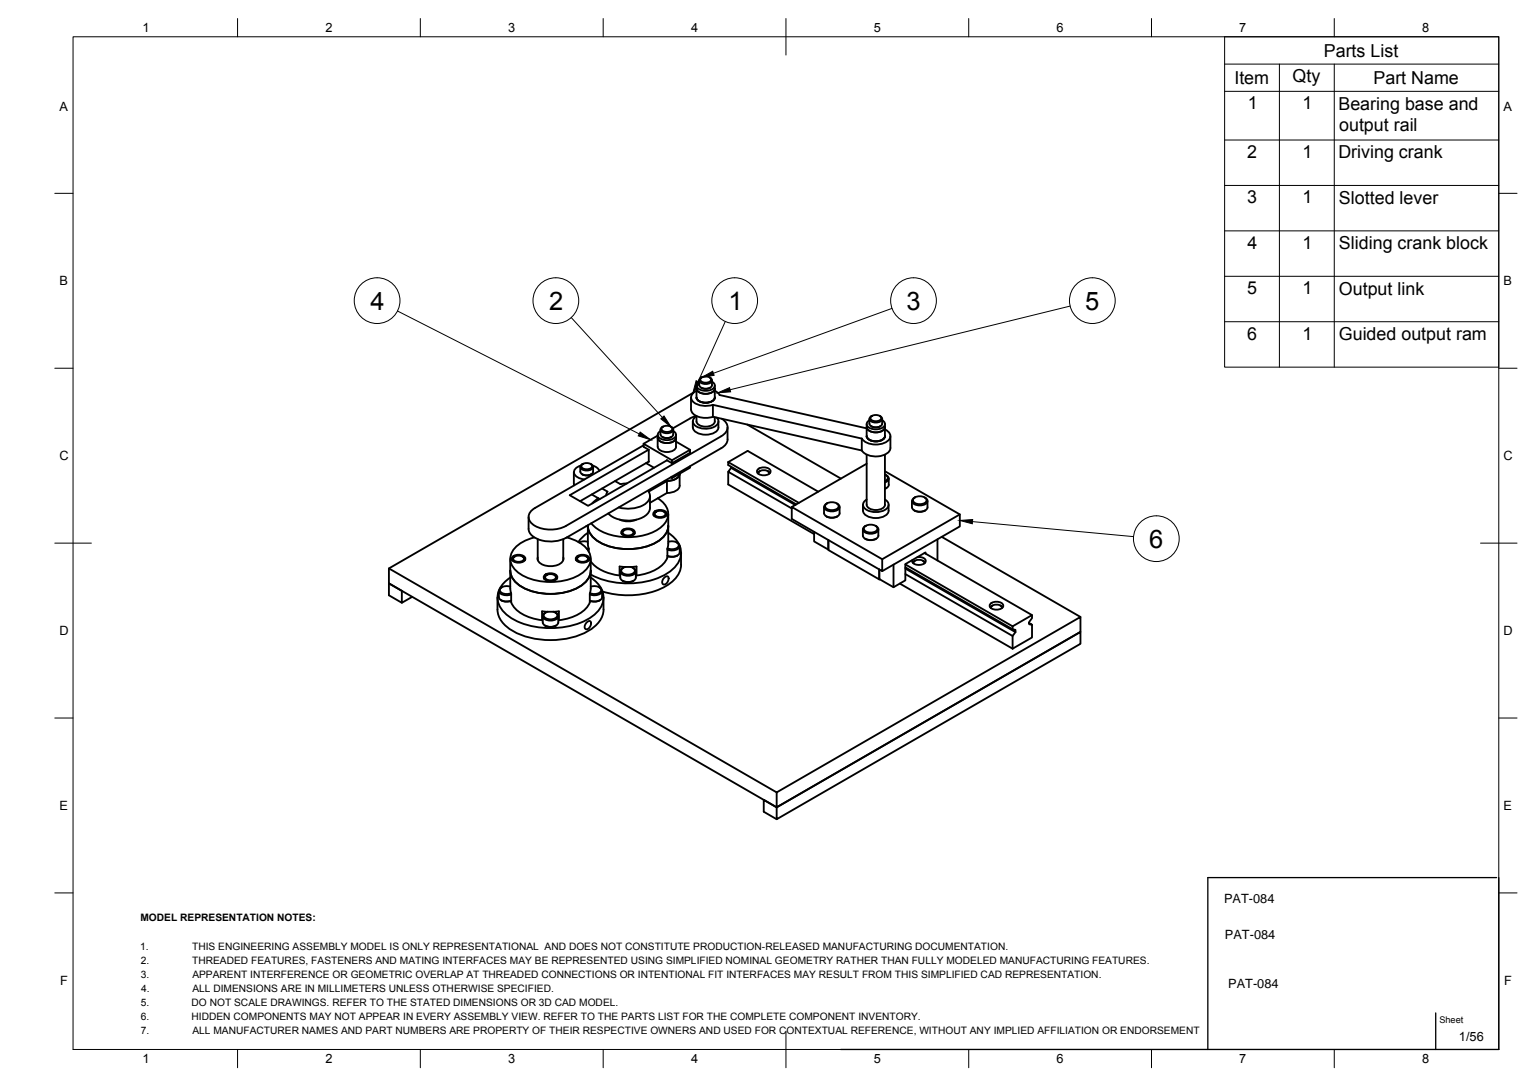
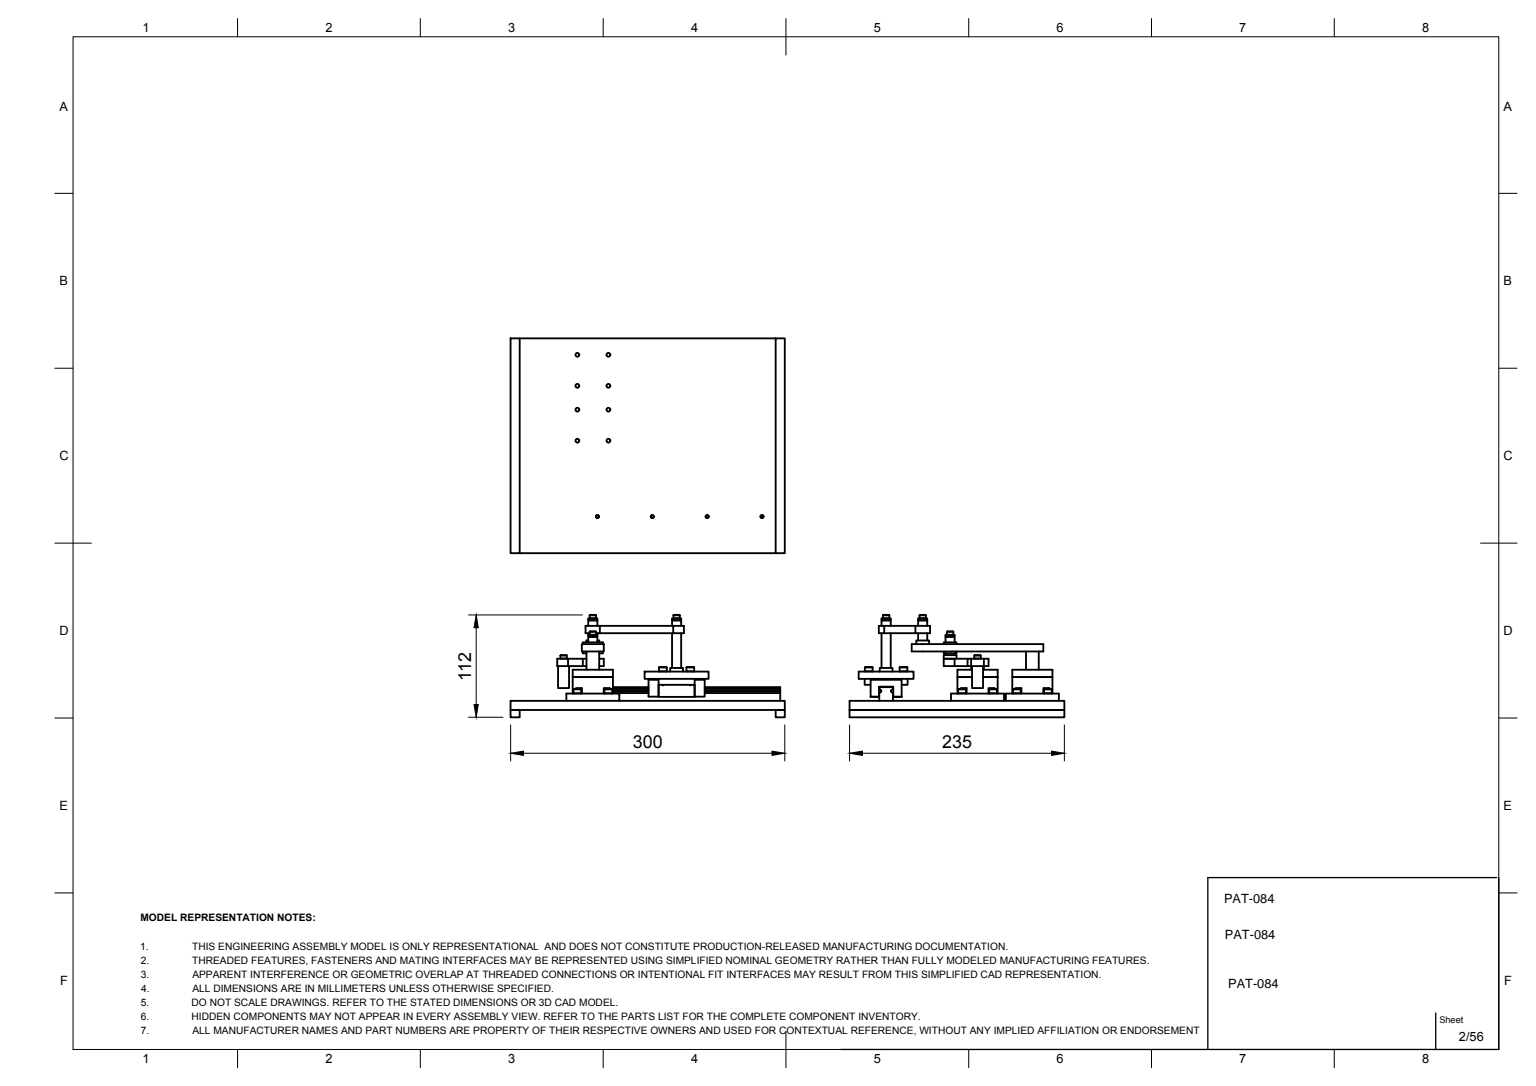
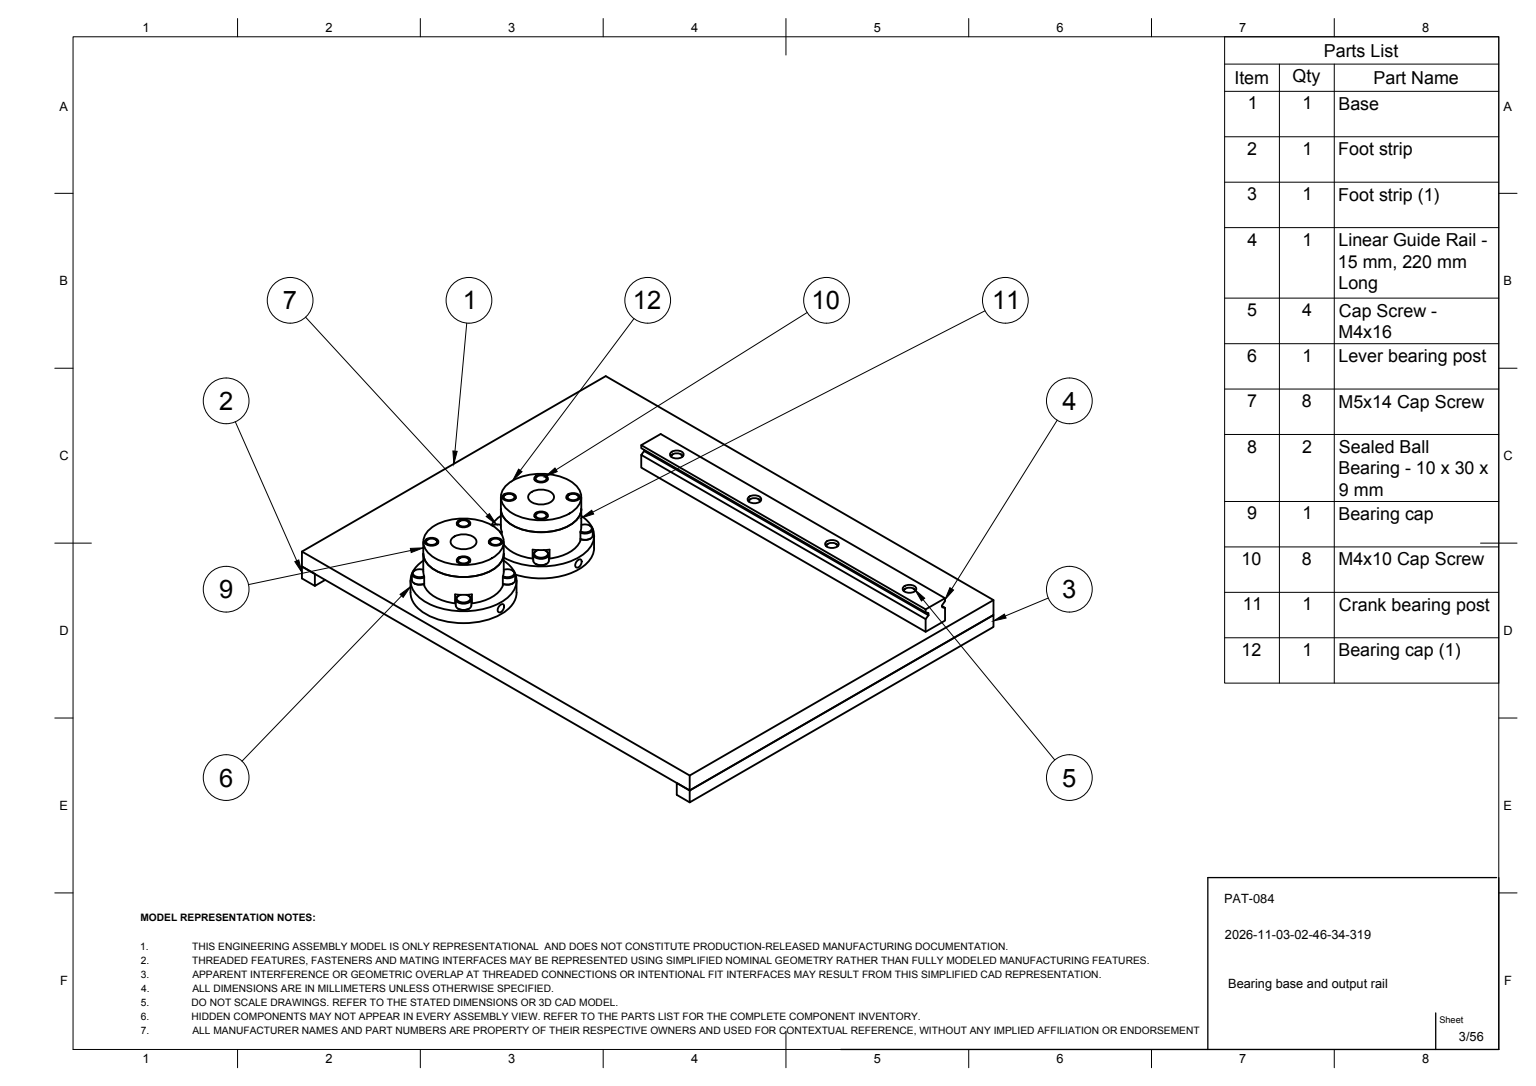
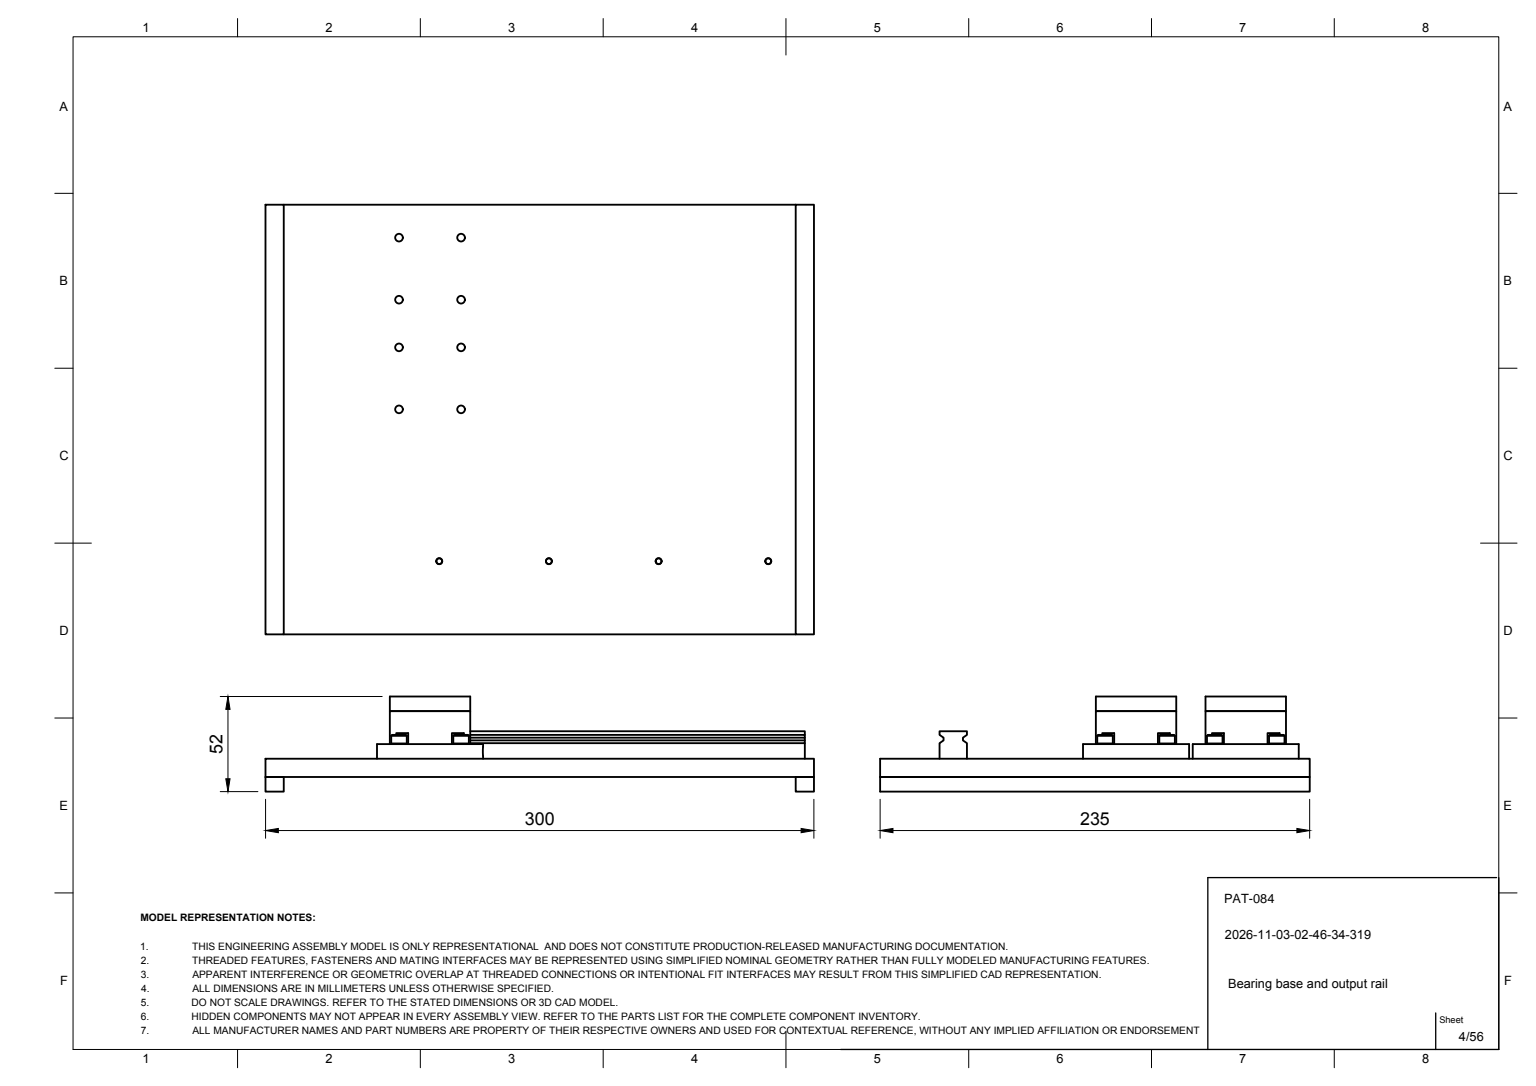
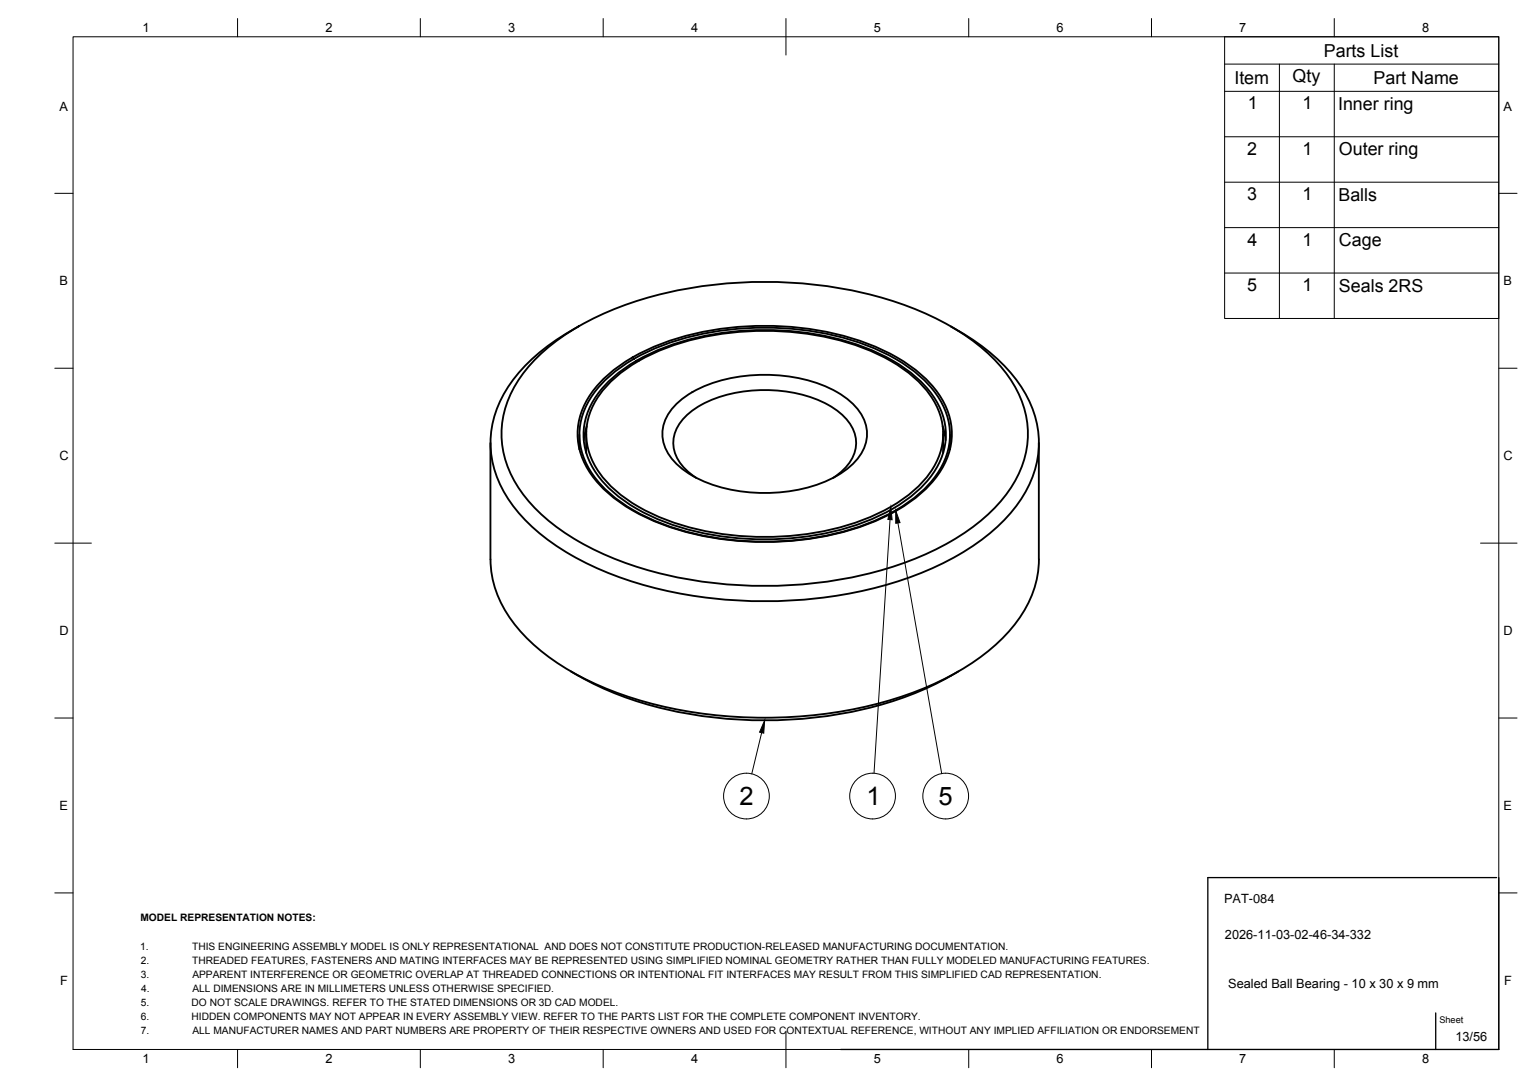
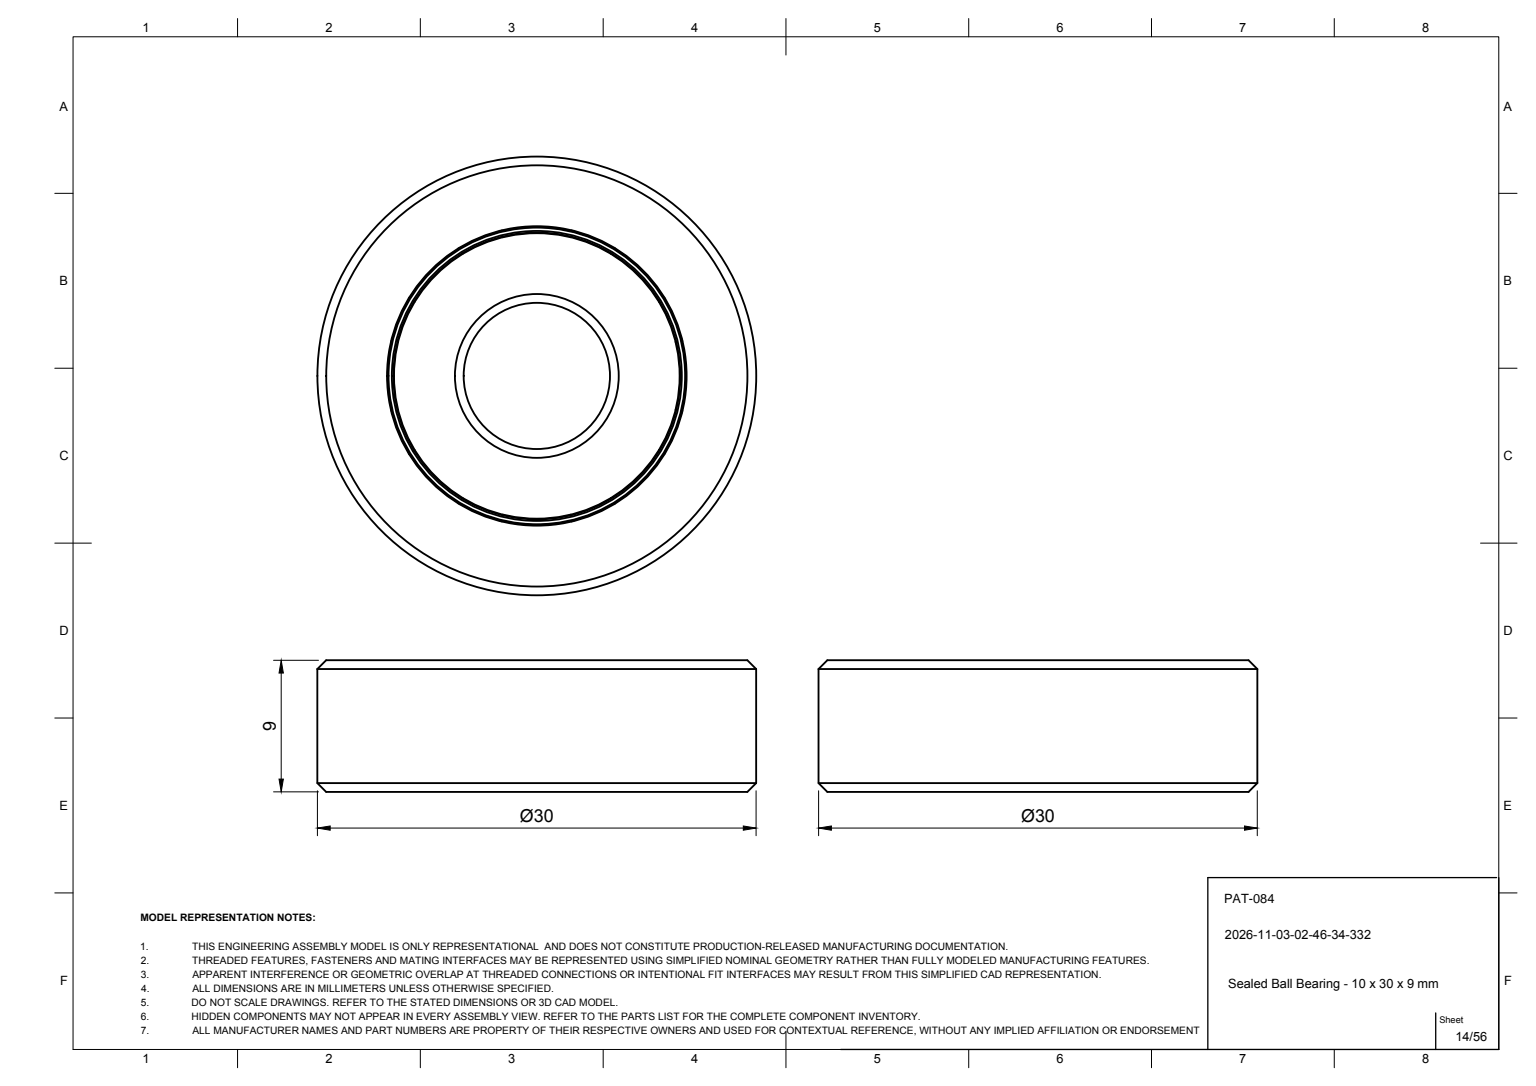
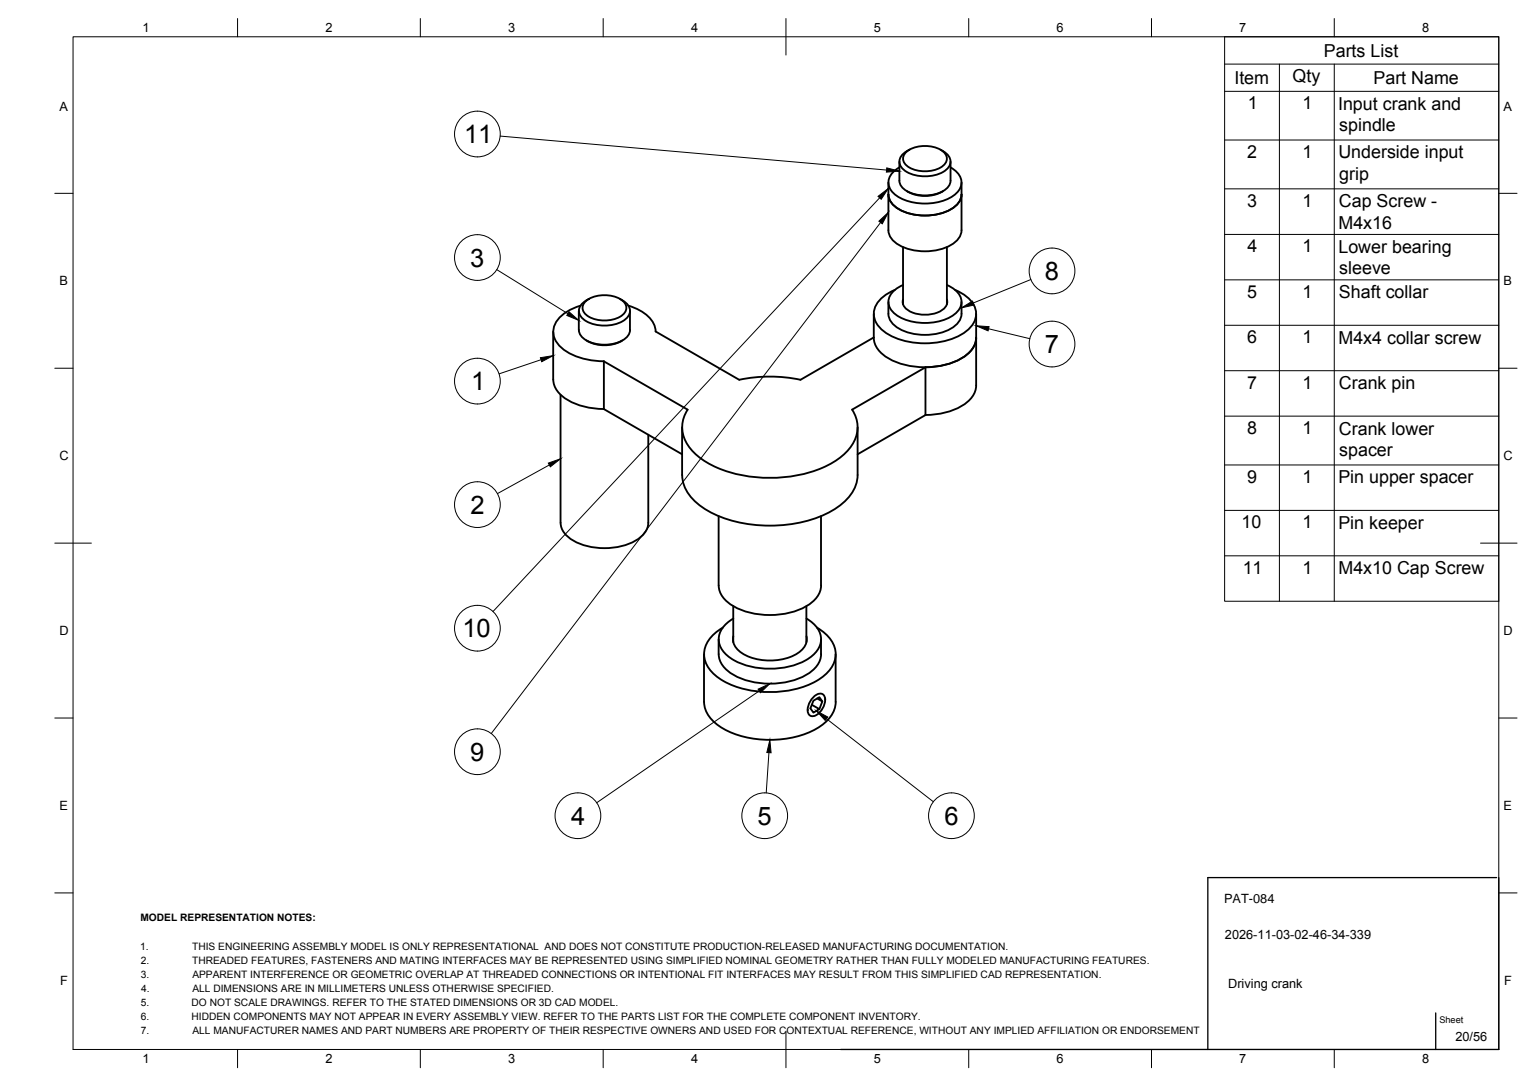
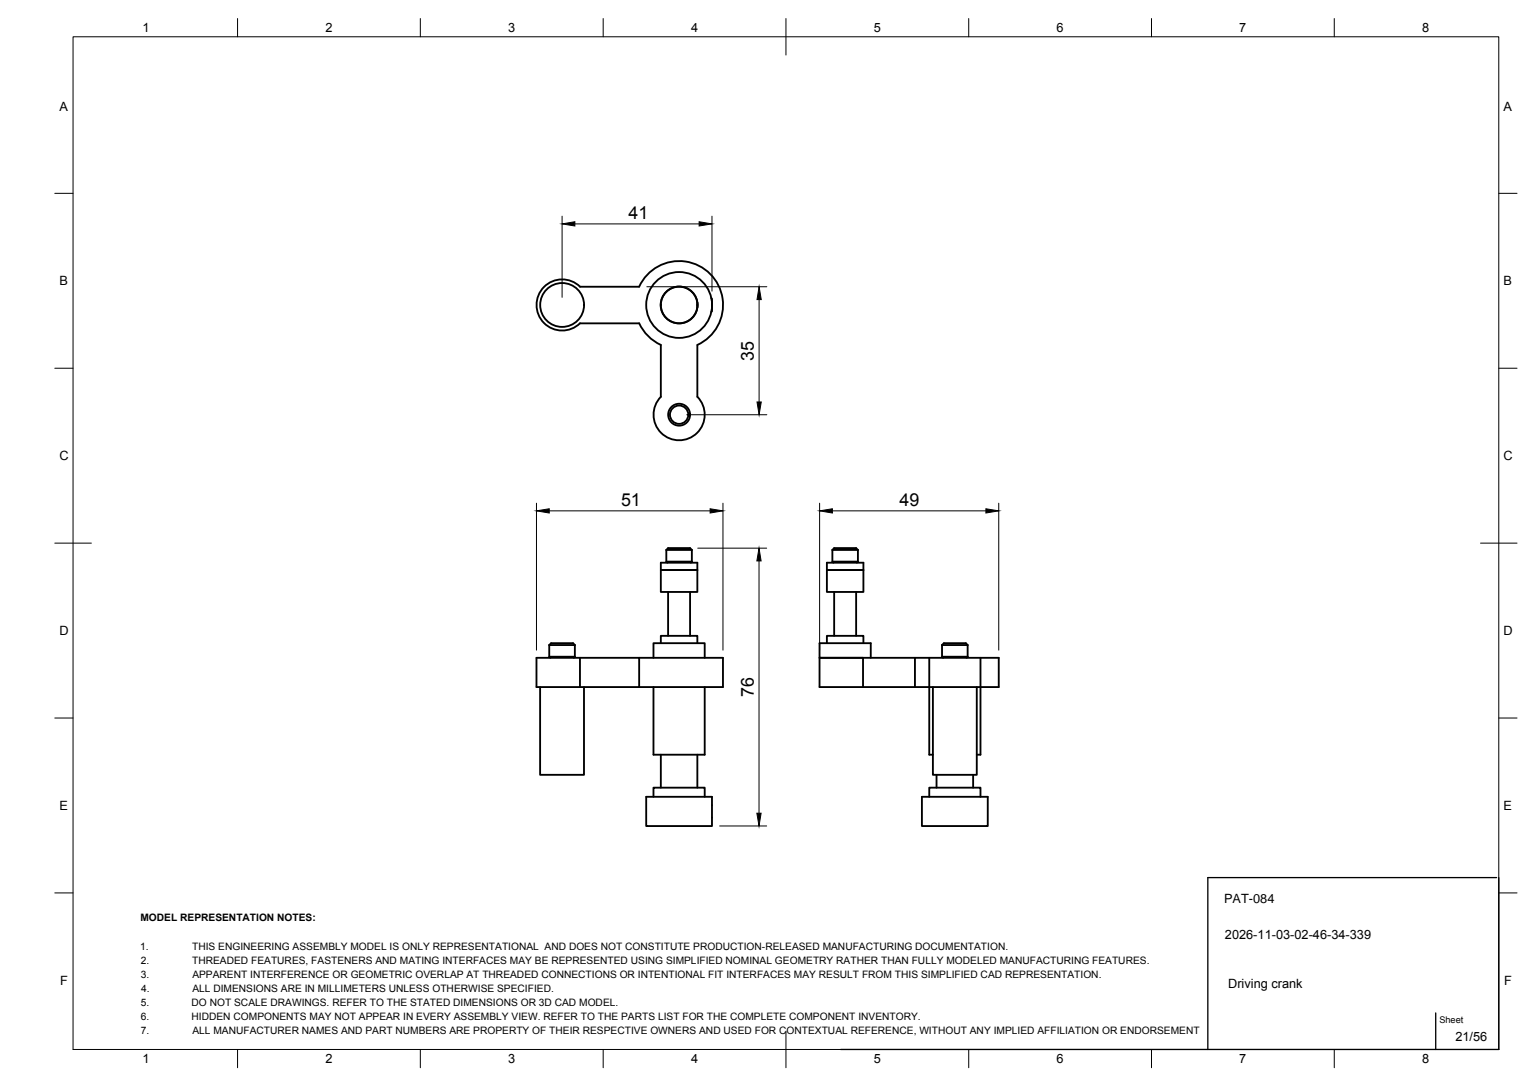
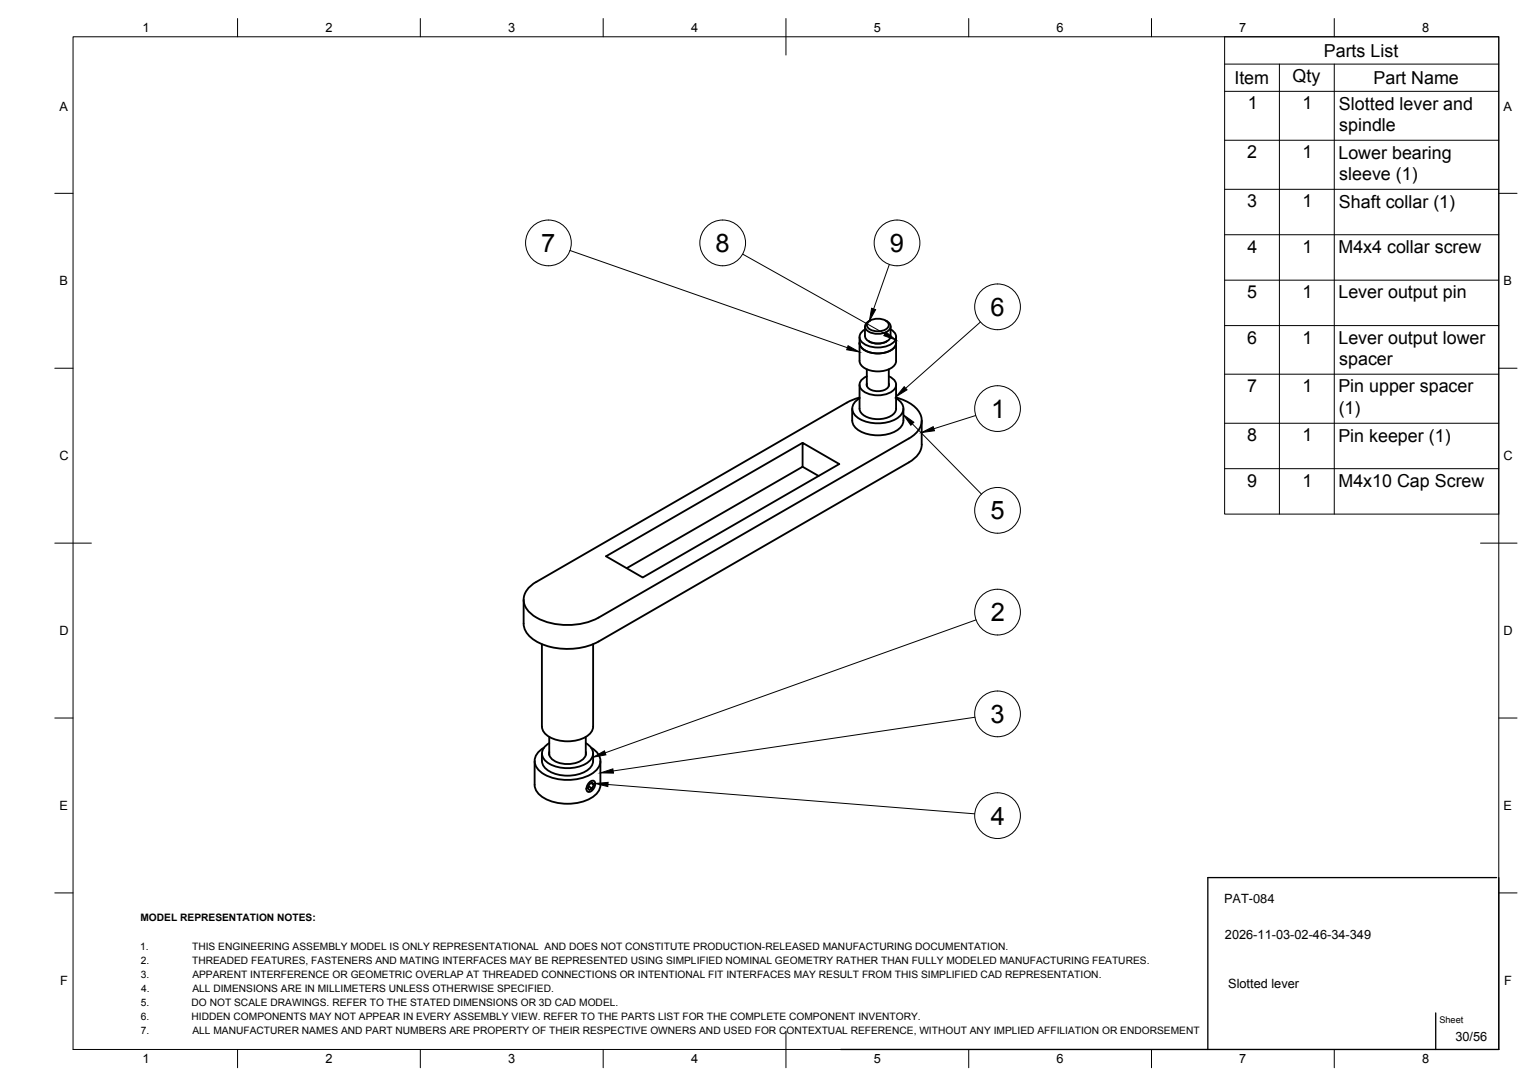
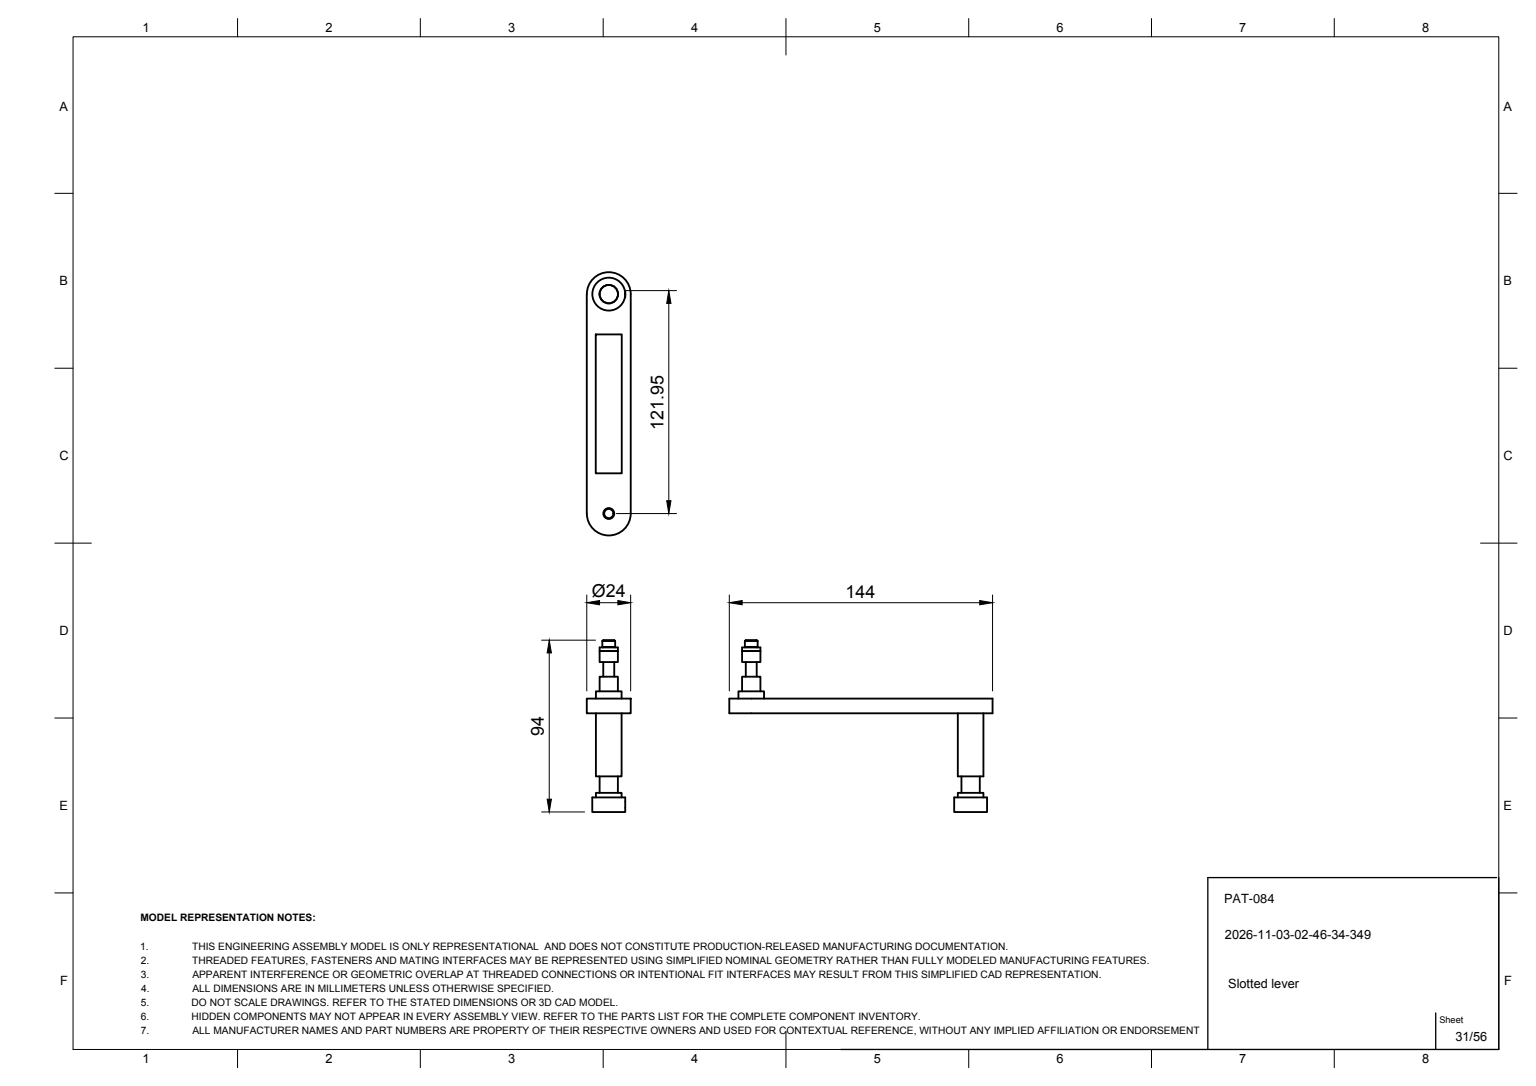
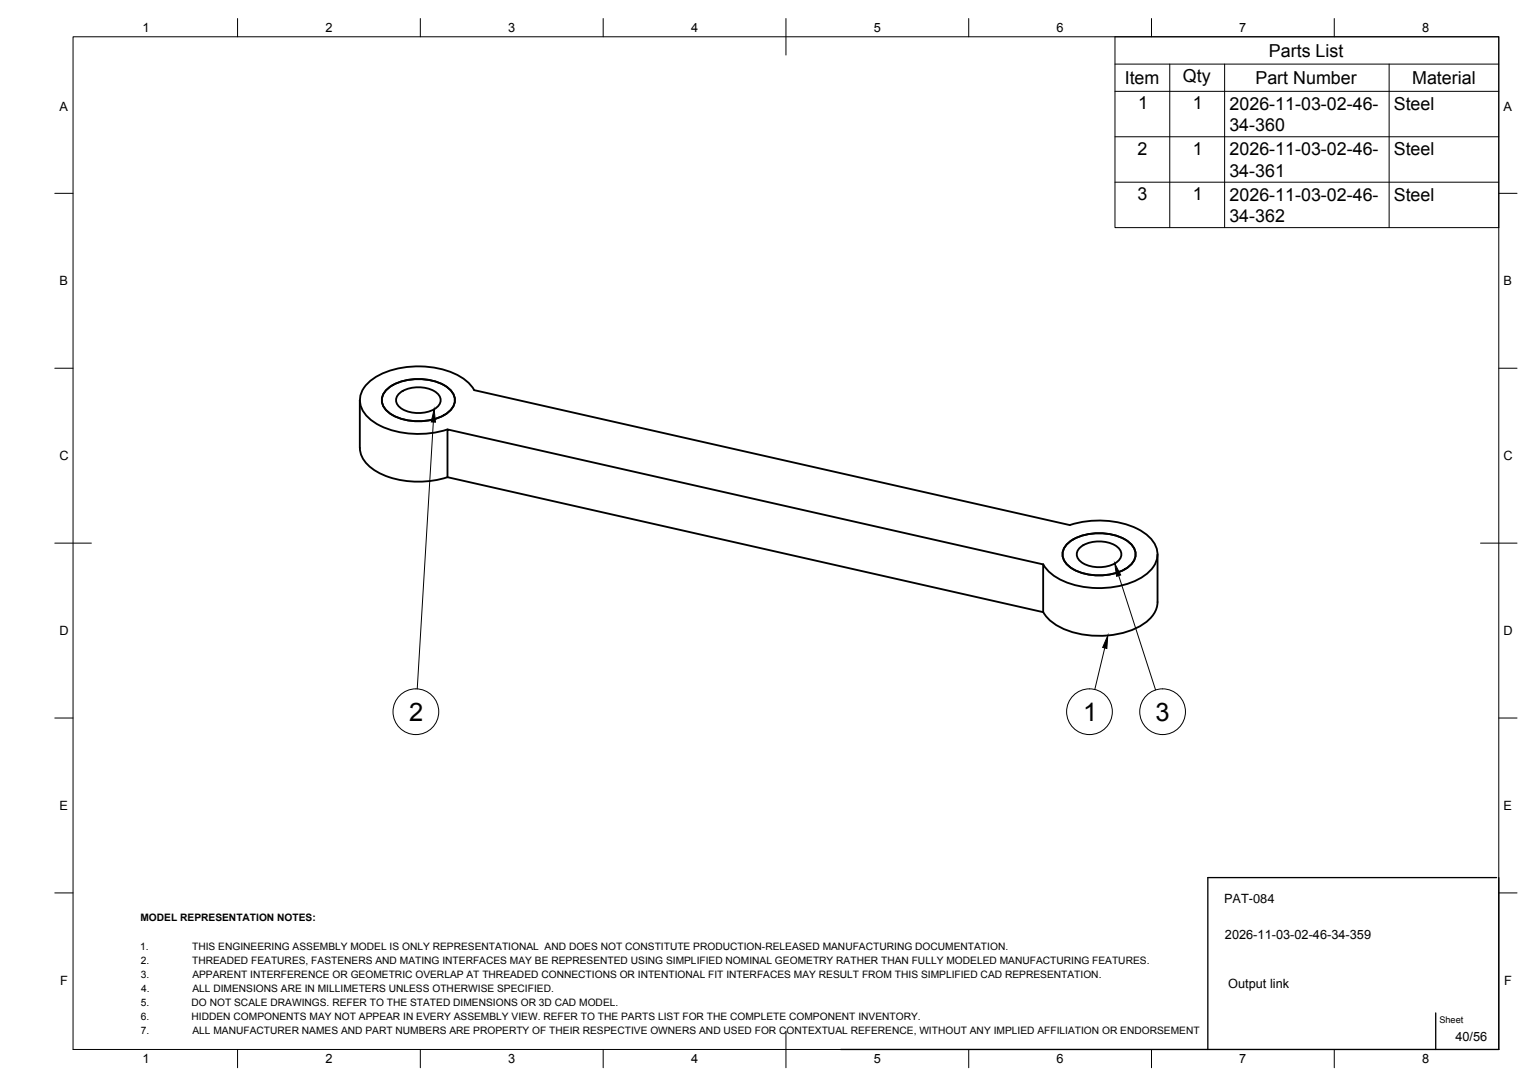
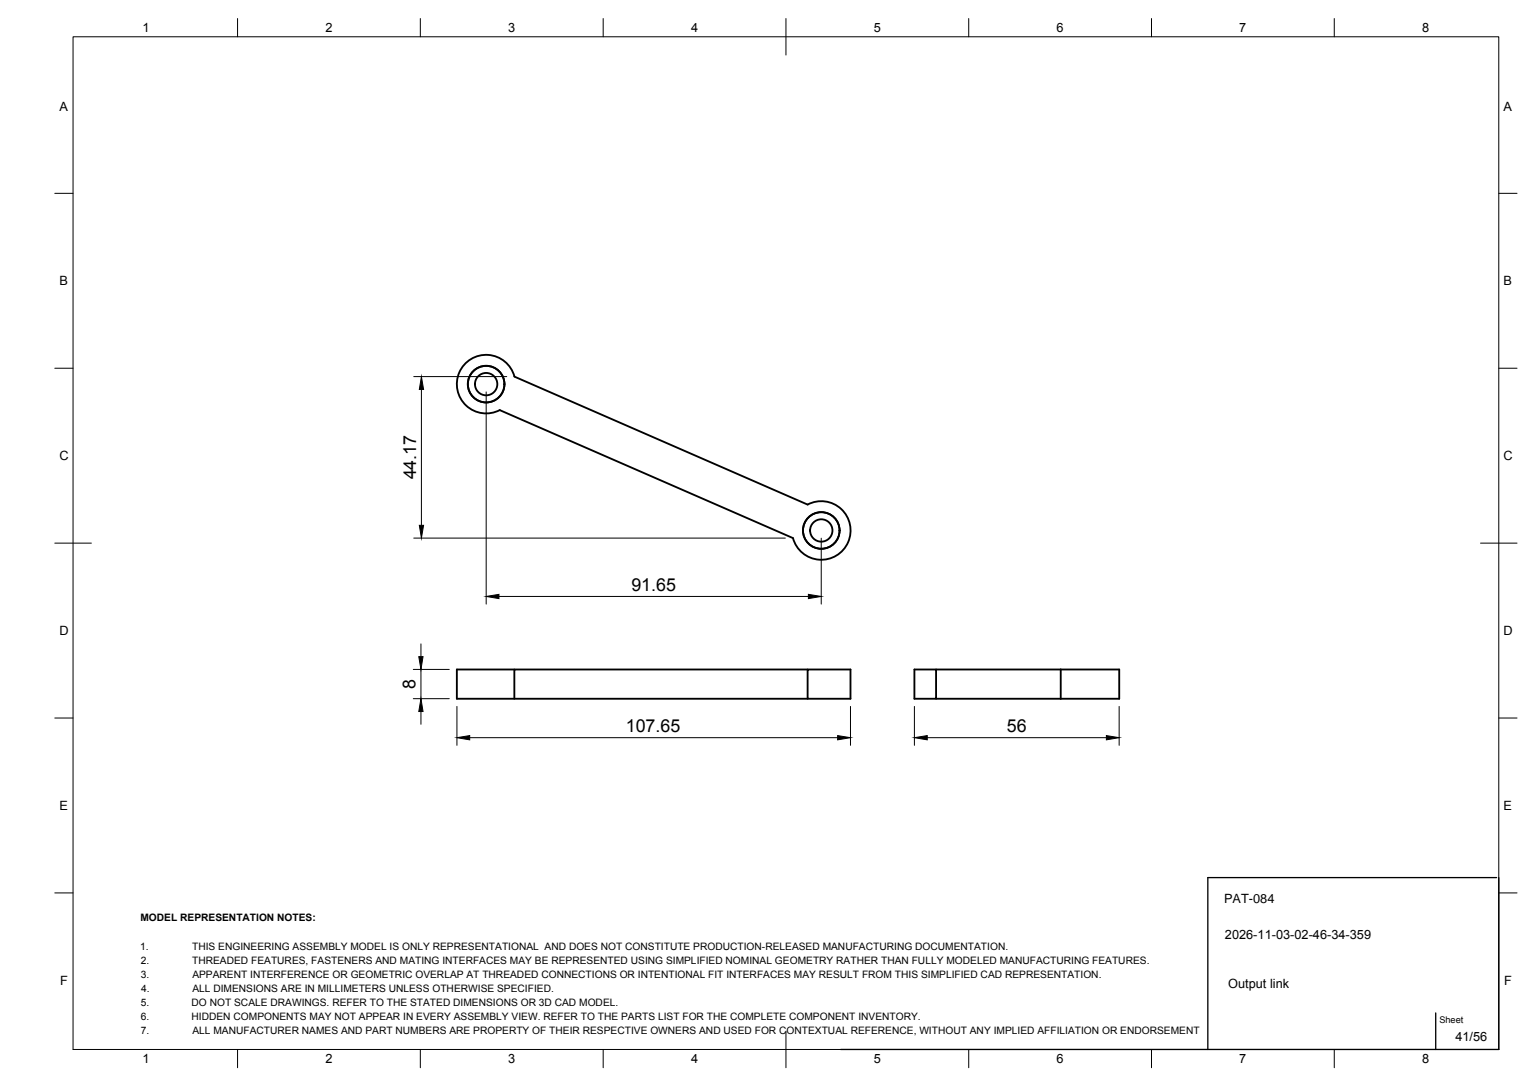
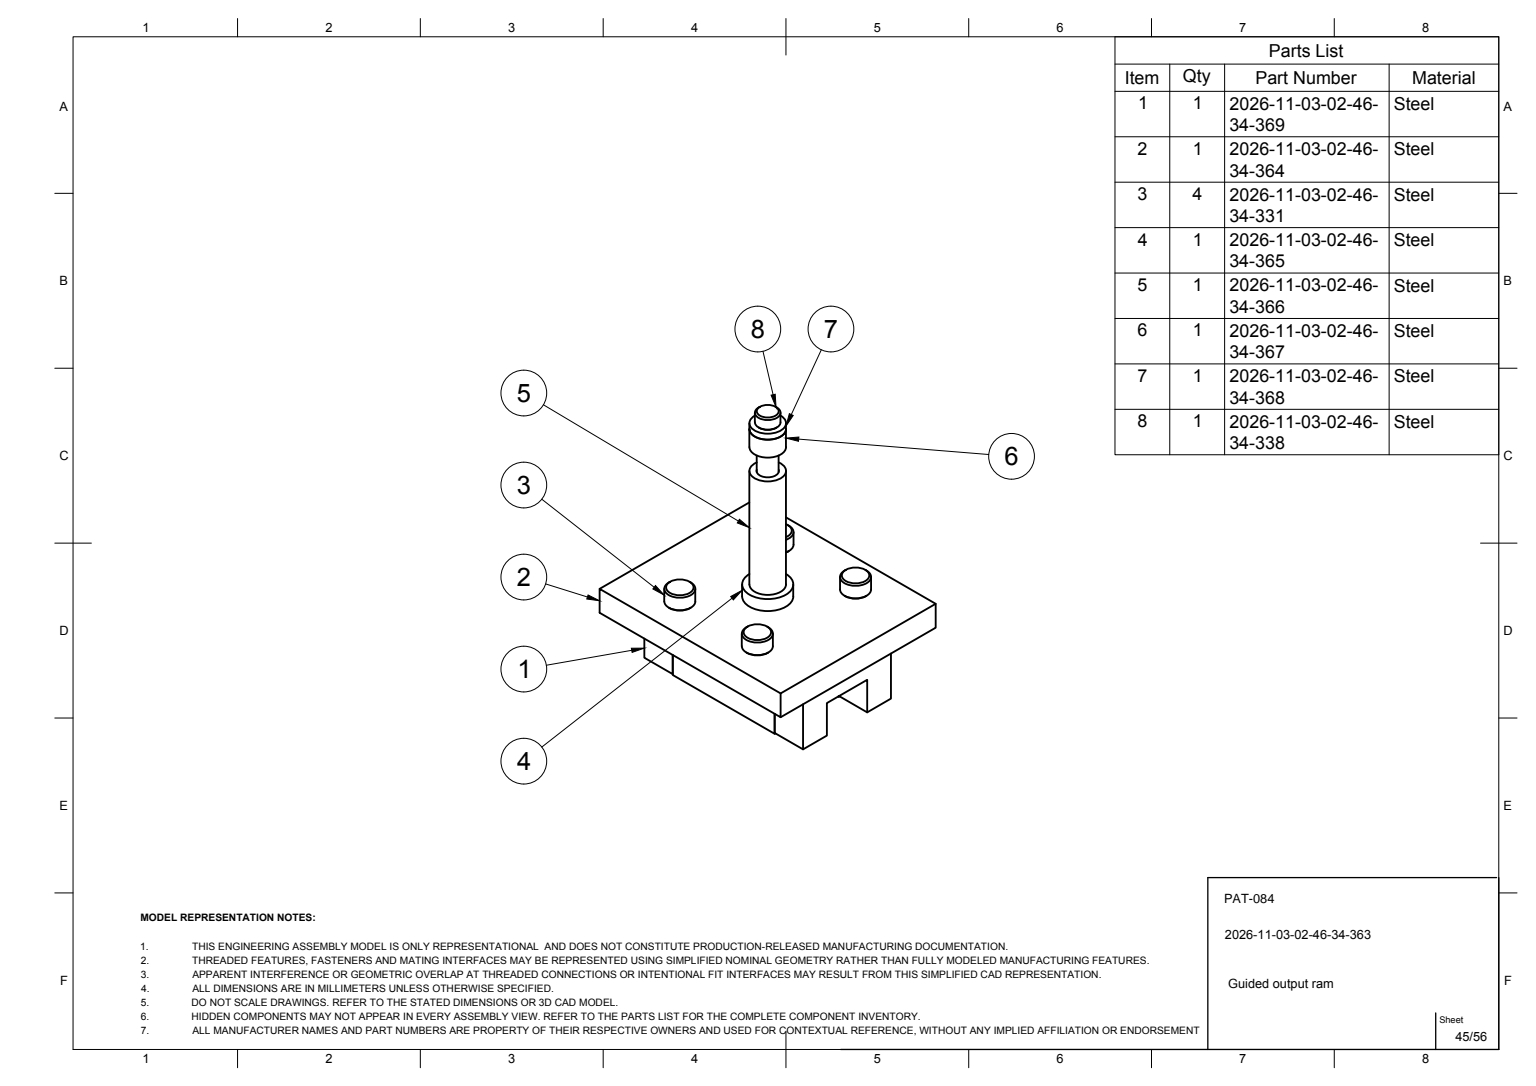
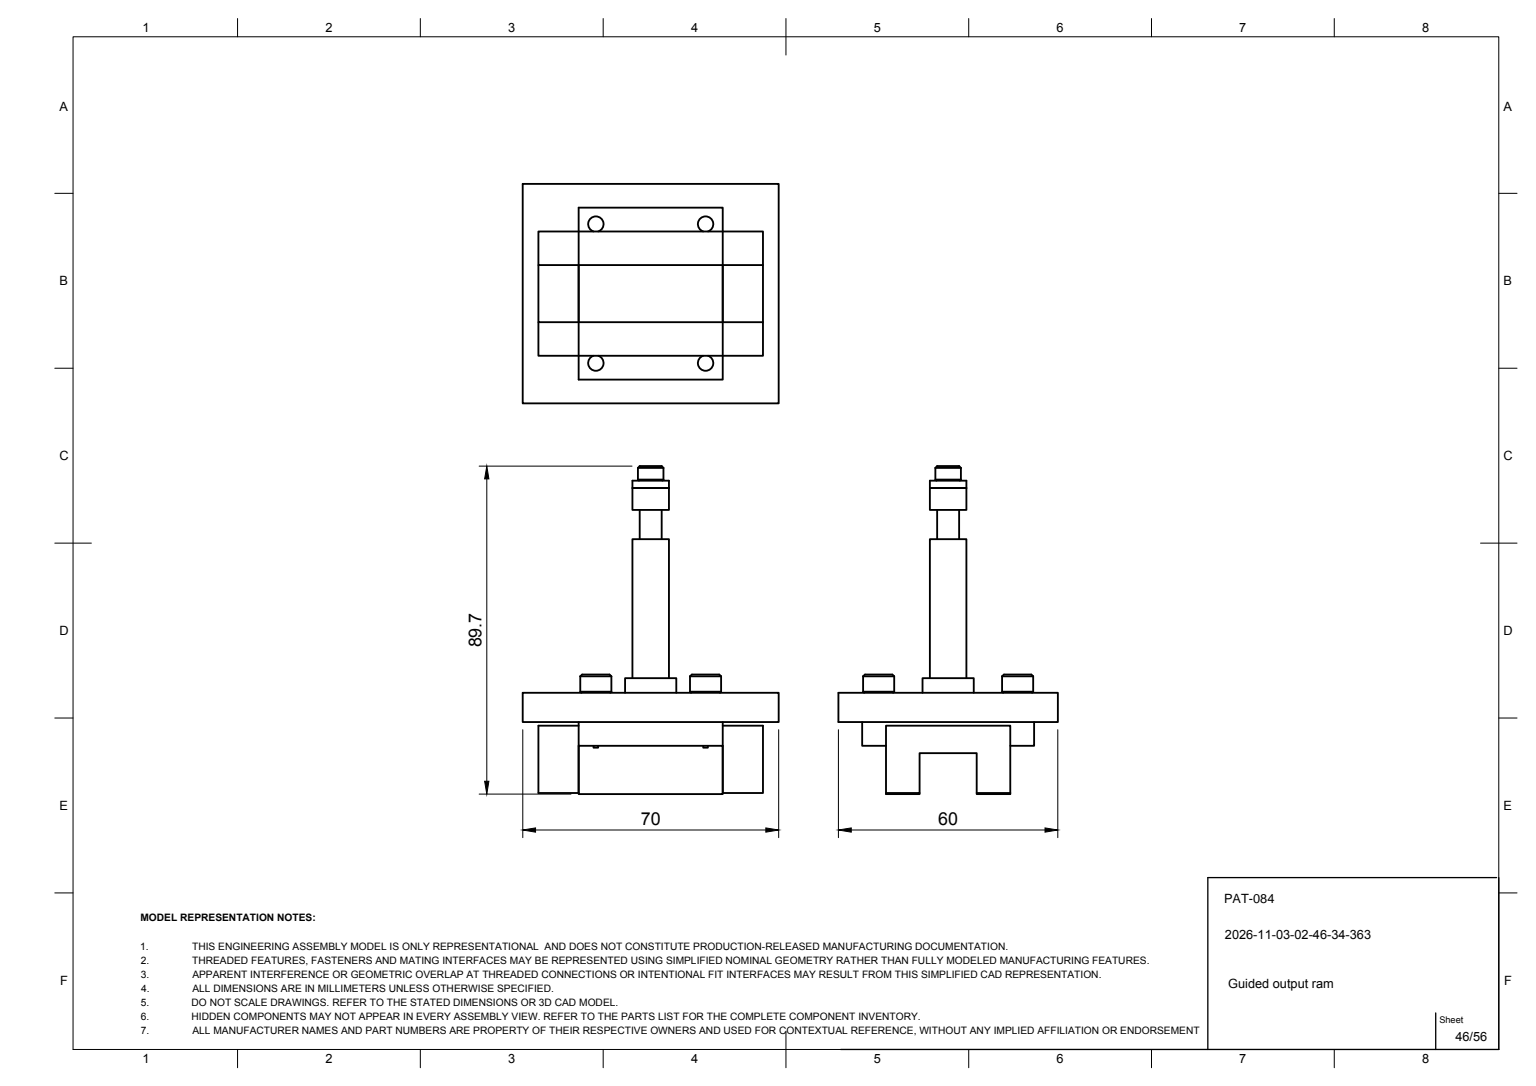
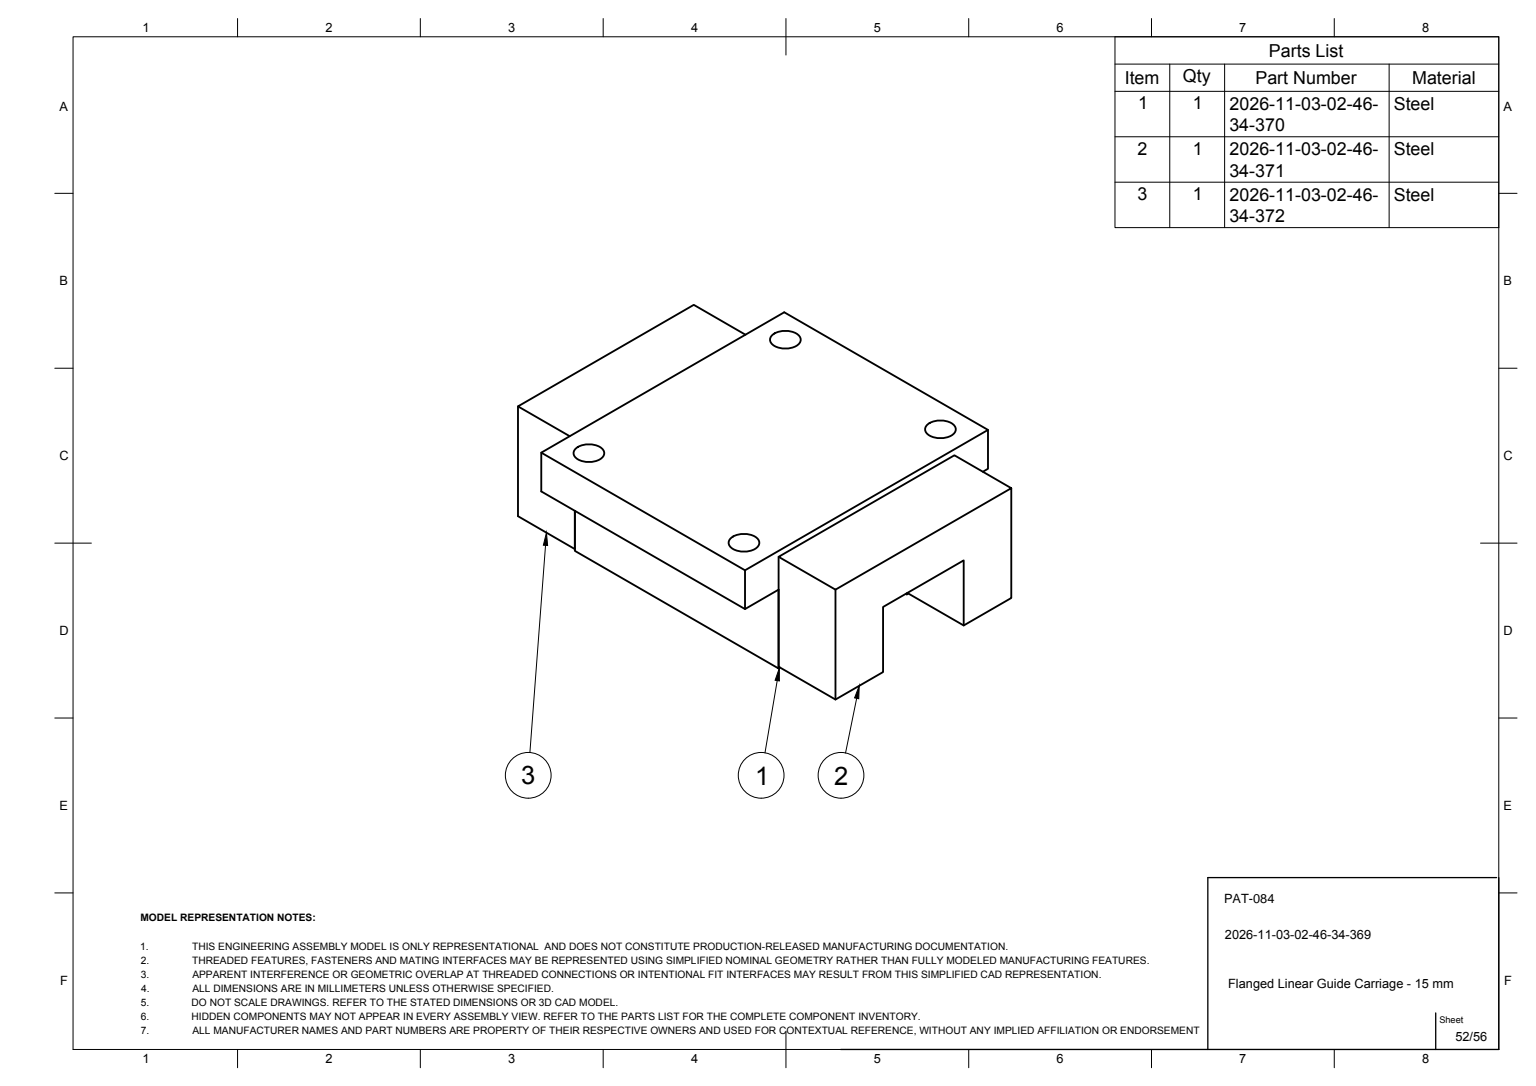
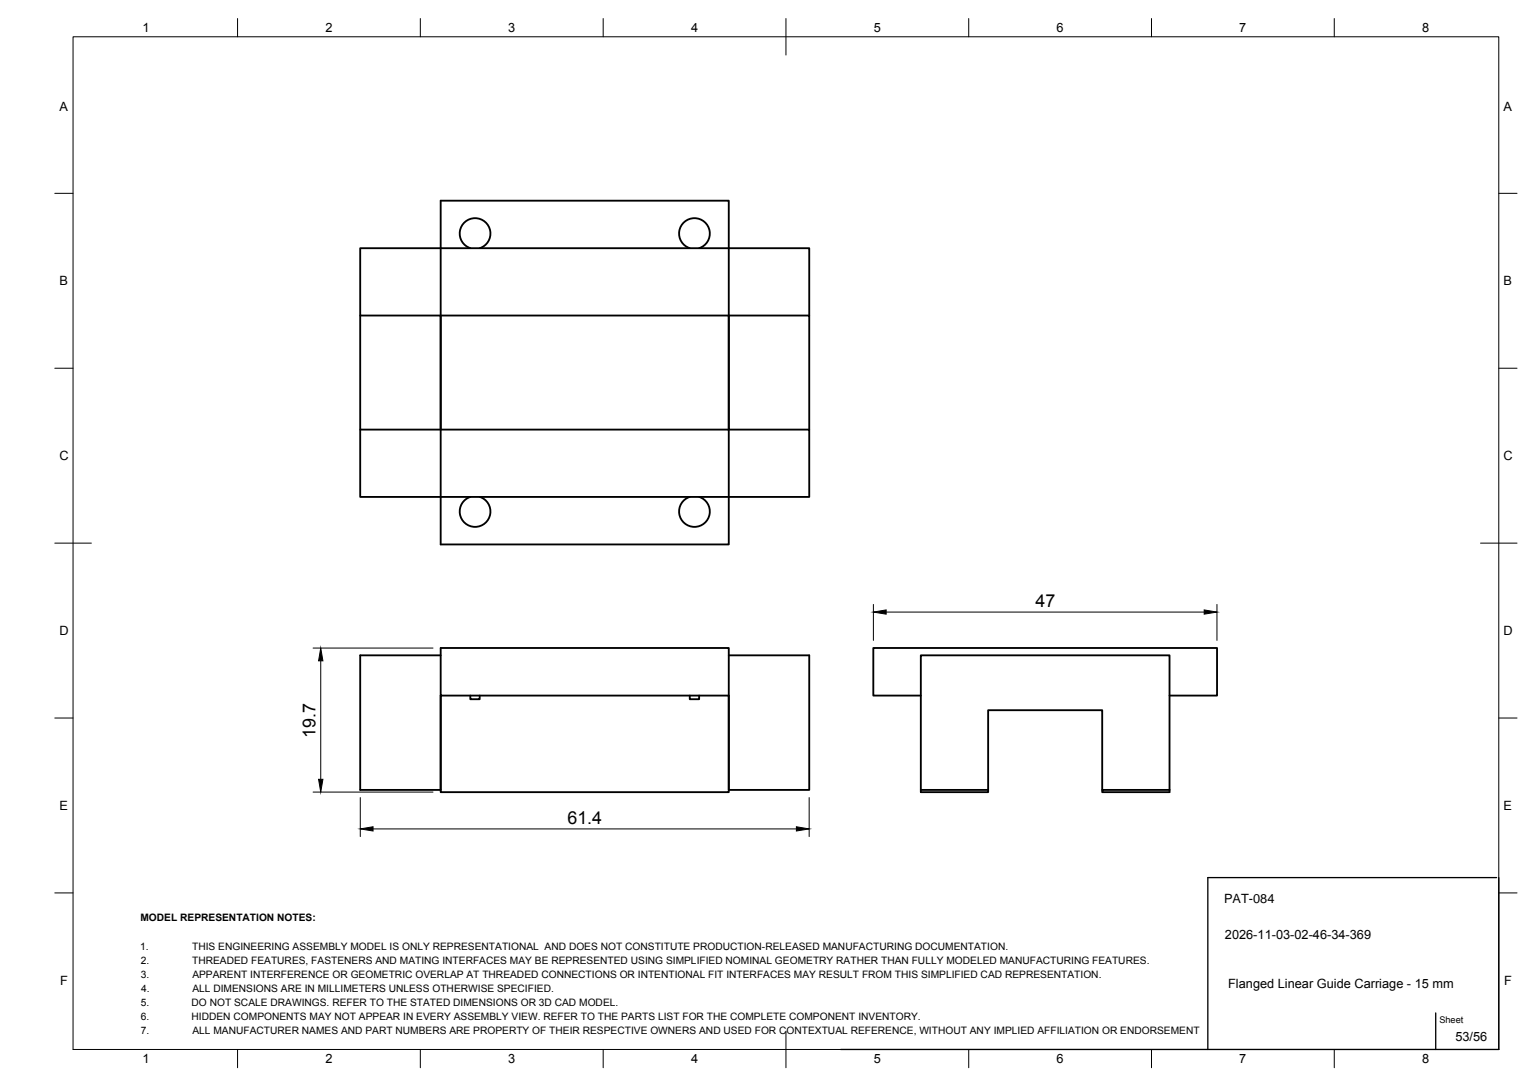
ISO-10303-21;
HEADER;
/* Generated by software containing ST-Developer
 * from STEP Tools, Inc. (www.steptools.com) 
 */

FILE_DESCRIPTION(
/* description */ ('Quick-return (Whitworth) mechanism'),
/* implementation_level */ '2;1');

FILE_NAME(
/* name */ 'PAT-084',
/* time_stamp */ '2026-10-28T03:25:57-07:00',
/* author */ (''),
/* organization */ (''),
/* preprocessor_version */ 'ST-DEVELOPER v20.2',
/* originating_system */ 'Autodesk Translation Framework v15.17.0.0',
/* authorisation */ '');

FILE_SCHEMA (('AUTOMOTIVE_DESIGN { 1 0 10303 214 3 1 1 }'));
ENDSEC;

DATA;
#10=MECHANICAL_DESIGN_GEOMETRIC_PRESENTATION_REPRESENTATION('',(#490,#491,
#492,#493,#494,#495,#496,#497,#498,#499,#500,#501,#502,#503,#504,#505,#506,
#507,#508,#509,#510,#511,#512,#513,#514,#515,#516,#517,#518,#519,#520,#521,
#522,#523,#524,#525,#526,#527,#528,#529,#530,#531,#532,#533,#534,#535,#536,
#537,#538,#539,#540,#541),#14878);
#11=ORIENTED_CLOSED_SHELL('',*,#7874,.F.);
#12=ORIENTED_CLOSED_SHELL('',*,#7895,.F.);
#13=ORIENTED_CLOSED_SHELL('',*,#7897,.F.);
#14=BREP_WITH_VOIDS('Body1',#7873,(#11));
#15=BREP_WITH_VOIDS('Body1',#7896,(#12));
#16=BREP_WITH_VOIDS('Body1',#7898,(#13));
#17=ITEM_DEFINED_TRANSFORMATION($,$,#8709,#8837);
#18=ITEM_DEFINED_TRANSFORMATION($,$,#8729,#8838);
#19=ITEM_DEFINED_TRANSFORMATION($,$,#8749,#8839);
#20=ITEM_DEFINED_TRANSFORMATION($,$,#8766,#8840);
#21=ITEM_DEFINED_TRANSFORMATION($,$,#8820,#8841);
#22=ITEM_DEFINED_TRANSFORMATION($,$,#9091,#9109);
#23=ITEM_DEFINED_TRANSFORMATION($,$,#9111,#9146);
#24=ITEM_DEFINED_TRANSFORMATION($,$,#9128,#9147);
#25=ITEM_DEFINED_TRANSFORMATION($,$,#9137,#9148);
#26=ITEM_DEFINED_TRANSFORMATION($,$,#9218,#9279);
#27=ITEM_DEFINED_TRANSFORMATION($,$,#9257,#9280);
#28=ITEM_DEFINED_TRANSFORMATION($,$,#9268,#9281);
#29=ITEM_DEFINED_TRANSFORMATION($,$,#8386,#9330);
#30=ITEM_DEFINED_TRANSFORMATION($,$,#8429,#9331);
#31=ITEM_DEFINED_TRANSFORMATION($,$,#8436,#9332);
#32=ITEM_DEFINED_TRANSFORMATION($,$,#8443,#9333);
#33=ITEM_DEFINED_TRANSFORMATION($,$,#8513,#9334);
#34=ITEM_DEFINED_TRANSFORMATION($,$,#8554,#9335);
#35=ITEM_DEFINED_TRANSFORMATION($,$,#8624,#9336);
#36=ITEM_DEFINED_TRANSFORMATION($,$,#8665,#9337);
#37=ITEM_DEFINED_TRANSFORMATION($,$,#8954,#9338);
#38=ITEM_DEFINED_TRANSFORMATION($,$,#8954,#9339);
#39=ITEM_DEFINED_TRANSFORMATION($,$,#8954,#9340);
#40=ITEM_DEFINED_TRANSFORMATION($,$,#8954,#9341);
#41=ITEM_DEFINED_TRANSFORMATION($,$,#9282,#9342);
#42=ITEM_DEFINED_TRANSFORMATION($,$,#9282,#9343);
#43=ITEM_DEFINED_TRANSFORMATION($,$,#9282,#9344);
#44=ITEM_DEFINED_TRANSFORMATION($,$,#9282,#9345);
#45=ITEM_DEFINED_TRANSFORMATION($,$,#8708,#9346);
#46=ITEM_DEFINED_TRANSFORMATION($,$,#9306,#9347);
#47=ITEM_DEFINED_TRANSFORMATION($,$,#9306,#9348);
#48=ITEM_DEFINED_TRANSFORMATION($,$,#9306,#9349);
#49=ITEM_DEFINED_TRANSFORMATION($,$,#9306,#9350);
#50=ITEM_DEFINED_TRANSFORMATION($,$,#9282,#9351);
#51=ITEM_DEFINED_TRANSFORMATION($,$,#9282,#9352);
#52=ITEM_DEFINED_TRANSFORMATION($,$,#9282,#9353);
#53=ITEM_DEFINED_TRANSFORMATION($,$,#9282,#9354);
#54=ITEM_DEFINED_TRANSFORMATION($,$,#8708,#9355);
#55=ITEM_DEFINED_TRANSFORMATION($,$,#9306,#9356);
#56=ITEM_DEFINED_TRANSFORMATION($,$,#9306,#9357);
#57=ITEM_DEFINED_TRANSFORMATION($,$,#9306,#9358);
#58=ITEM_DEFINED_TRANSFORMATION($,$,#9306,#9359);
#59=ITEM_DEFINED_TRANSFORMATION($,$,#8843,#9360);
#60=ITEM_DEFINED_TRANSFORMATION($,$,#8876,#9361);
#61=ITEM_DEFINED_TRANSFORMATION($,$,#8886,#9362);
#62=ITEM_DEFINED_TRANSFORMATION($,$,#8895,#9363);
#63=ITEM_DEFINED_TRANSFORMATION($,$,#8909,#9364);
#64=ITEM_DEFINED_TRANSFORMATION($,$,#8927,#9365);
#65=ITEM_DEFINED_TRANSFORMATION($,$,#8936,#9366);
#66=ITEM_DEFINED_TRANSFORMATION($,$,#8945,#9367);
#67=ITEM_DEFINED_TRANSFORMATION($,$,#8954,#9368);
#68=ITEM_DEFINED_TRANSFORMATION($,$,#9075,#9369);
#69=ITEM_DEFINED_TRANSFORMATION($,$,#9306,#9370);
#70=ITEM_DEFINED_TRANSFORMATION($,$,#8981,#9371);
#71=ITEM_DEFINED_TRANSFORMATION($,$,#9007,#9372);
#72=ITEM_DEFINED_TRANSFORMATION($,$,#9016,#9373);
#73=ITEM_DEFINED_TRANSFORMATION($,$,#9030,#9374);
#74=ITEM_DEFINED_TRANSFORMATION($,$,#9048,#9375);
#75=ITEM_DEFINED_TRANSFORMATION($,$,#9057,#9376);
#76=ITEM_DEFINED_TRANSFORMATION($,$,#9066,#9377);
#77=ITEM_DEFINED_TRANSFORMATION($,$,#9075,#9378);
#78=ITEM_DEFINED_TRANSFORMATION($,$,#9306,#9379);
#79=ITEM_DEFINED_TRANSFORMATION($,$,#9150,#9380);
#80=ITEM_DEFINED_TRANSFORMATION($,$,#9172,#9381);
#81=ITEM_DEFINED_TRANSFORMATION($,$,#9190,#9382);
#82=ITEM_DEFINED_TRANSFORMATION($,$,#9199,#9383);
#83=ITEM_DEFINED_TRANSFORMATION($,$,#9208,#9384);
#84=ITEM_DEFINED_TRANSFORMATION($,$,#9217,#9385);
#85=ITEM_DEFINED_TRANSFORMATION($,$,#9282,#9386);
#86=ITEM_DEFINED_TRANSFORMATION($,$,#9282,#9387);
#87=ITEM_DEFINED_TRANSFORMATION($,$,#9282,#9388);
#88=ITEM_DEFINED_TRANSFORMATION($,$,#9282,#9389);
#89=ITEM_DEFINED_TRANSFORMATION($,$,#9306,#9390);
#90=ITEM_DEFINED_TRANSFORMATION($,$,#8385,#9391);
#91=ITEM_DEFINED_TRANSFORMATION($,$,#8842,#9392);
#92=ITEM_DEFINED_TRANSFORMATION($,$,#8980,#9393);
#93=ITEM_DEFINED_TRANSFORMATION($,$,#9090,#9394);
#94=ITEM_DEFINED_TRANSFORMATION($,$,#9110,#9395);
#95=ITEM_DEFINED_TRANSFORMATION($,$,#9149,#9396);
#96=(
REPRESENTATION_RELATIONSHIP($,$,#15079,#15078)
REPRESENTATION_RELATIONSHIP_WITH_TRANSFORMATION(#17)
SHAPE_REPRESENTATION_RELATIONSHIP()
);
#97=(
REPRESENTATION_RELATIONSHIP($,$,#15080,#15078)
REPRESENTATION_RELATIONSHIP_WITH_TRANSFORMATION(#18)
SHAPE_REPRESENTATION_RELATIONSHIP()
);
#98=(
REPRESENTATION_RELATIONSHIP($,$,#15081,#15078)
REPRESENTATION_RELATIONSHIP_WITH_TRANSFORMATION(#19)
SHAPE_REPRESENTATION_RELATIONSHIP()
);
#99=(
REPRESENTATION_RELATIONSHIP($,$,#15082,#15078)
REPRESENTATION_RELATIONSHIP_WITH_TRANSFORMATION(#20)
SHAPE_REPRESENTATION_RELATIONSHIP()
);
#100=(
REPRESENTATION_RELATIONSHIP($,$,#15083,#15078)
REPRESENTATION_RELATIONSHIP_WITH_TRANSFORMATION(#21)
SHAPE_REPRESENTATION_RELATIONSHIP()
);
#101=(
REPRESENTATION_RELATIONSHIP($,$,#15104,#15103)
REPRESENTATION_RELATIONSHIP_WITH_TRANSFORMATION(#22)
SHAPE_REPRESENTATION_RELATIONSHIP()
);
#102=(
REPRESENTATION_RELATIONSHIP($,$,#15106,#15105)
REPRESENTATION_RELATIONSHIP_WITH_TRANSFORMATION(#23)
SHAPE_REPRESENTATION_RELATIONSHIP()
);
#103=(
REPRESENTATION_RELATIONSHIP($,$,#15107,#15105)
REPRESENTATION_RELATIONSHIP_WITH_TRANSFORMATION(#24)
SHAPE_REPRESENTATION_RELATIONSHIP()
);
#104=(
REPRESENTATION_RELATIONSHIP($,$,#15108,#15105)
REPRESENTATION_RELATIONSHIP_WITH_TRANSFORMATION(#25)
SHAPE_REPRESENTATION_RELATIONSHIP()
);
#105=(
REPRESENTATION_RELATIONSHIP($,$,#15116,#15115)
REPRESENTATION_RELATIONSHIP_WITH_TRANSFORMATION(#26)
SHAPE_REPRESENTATION_RELATIONSHIP()
);
#106=(
REPRESENTATION_RELATIONSHIP($,$,#15117,#15115)
REPRESENTATION_RELATIONSHIP_WITH_TRANSFORMATION(#27)
SHAPE_REPRESENTATION_RELATIONSHIP()
);
#107=(
REPRESENTATION_RELATIONSHIP($,$,#15118,#15115)
REPRESENTATION_RELATIONSHIP_WITH_TRANSFORMATION(#28)
SHAPE_REPRESENTATION_RELATIONSHIP()
);
#108=(
REPRESENTATION_RELATIONSHIP($,$,#15070,#15069)
REPRESENTATION_RELATIONSHIP_WITH_TRANSFORMATION(#29)
SHAPE_REPRESENTATION_RELATIONSHIP()
);
#109=(
REPRESENTATION_RELATIONSHIP($,$,#15071,#15069)
REPRESENTATION_RELATIONSHIP_WITH_TRANSFORMATION(#30)
SHAPE_REPRESENTATION_RELATIONSHIP()
);
#110=(
REPRESENTATION_RELATIONSHIP($,$,#15072,#15069)
REPRESENTATION_RELATIONSHIP_WITH_TRANSFORMATION(#31)
SHAPE_REPRESENTATION_RELATIONSHIP()
);
#111=(
REPRESENTATION_RELATIONSHIP($,$,#15073,#15069)
REPRESENTATION_RELATIONSHIP_WITH_TRANSFORMATION(#32)
SHAPE_REPRESENTATION_RELATIONSHIP()
);
#112=(
REPRESENTATION_RELATIONSHIP($,$,#15074,#15069)
REPRESENTATION_RELATIONSHIP_WITH_TRANSFORMATION(#33)
SHAPE_REPRESENTATION_RELATIONSHIP()
);
#113=(
REPRESENTATION_RELATIONSHIP($,$,#15075,#15069)
REPRESENTATION_RELATIONSHIP_WITH_TRANSFORMATION(#34)
SHAPE_REPRESENTATION_RELATIONSHIP()
);
#114=(
REPRESENTATION_RELATIONSHIP($,$,#15076,#15069)
REPRESENTATION_RELATIONSHIP_WITH_TRANSFORMATION(#35)
SHAPE_REPRESENTATION_RELATIONSHIP()
);
#115=(
REPRESENTATION_RELATIONSHIP($,$,#15077,#15069)
REPRESENTATION_RELATIONSHIP_WITH_TRANSFORMATION(#36)
SHAPE_REPRESENTATION_RELATIONSHIP()
);
#116=(
REPRESENTATION_RELATIONSHIP($,$,#15093,#15069)
REPRESENTATION_RELATIONSHIP_WITH_TRANSFORMATION(#37)
SHAPE_REPRESENTATION_RELATIONSHIP()
);
#117=(
REPRESENTATION_RELATIONSHIP($,$,#15093,#15069)
REPRESENTATION_RELATIONSHIP_WITH_TRANSFORMATION(#38)
SHAPE_REPRESENTATION_RELATIONSHIP()
);
#118=(
REPRESENTATION_RELATIONSHIP($,$,#15093,#15069)
REPRESENTATION_RELATIONSHIP_WITH_TRANSFORMATION(#39)
SHAPE_REPRESENTATION_RELATIONSHIP()
);
#119=(
REPRESENTATION_RELATIONSHIP($,$,#15093,#15069)
REPRESENTATION_RELATIONSHIP_WITH_TRANSFORMATION(#40)
SHAPE_REPRESENTATION_RELATIONSHIP()
);
#120=(
REPRESENTATION_RELATIONSHIP($,$,#15119,#15069)
REPRESENTATION_RELATIONSHIP_WITH_TRANSFORMATION(#41)
SHAPE_REPRESENTATION_RELATIONSHIP()
);
#121=(
REPRESENTATION_RELATIONSHIP($,$,#15119,#15069)
REPRESENTATION_RELATIONSHIP_WITH_TRANSFORMATION(#42)
SHAPE_REPRESENTATION_RELATIONSHIP()
);
#122=(
REPRESENTATION_RELATIONSHIP($,$,#15119,#15069)
REPRESENTATION_RELATIONSHIP_WITH_TRANSFORMATION(#43)
SHAPE_REPRESENTATION_RELATIONSHIP()
);
#123=(
REPRESENTATION_RELATIONSHIP($,$,#15119,#15069)
REPRESENTATION_RELATIONSHIP_WITH_TRANSFORMATION(#44)
SHAPE_REPRESENTATION_RELATIONSHIP()
);
#124=(
REPRESENTATION_RELATIONSHIP($,$,#15078,#15069)
REPRESENTATION_RELATIONSHIP_WITH_TRANSFORMATION(#45)
SHAPE_REPRESENTATION_RELATIONSHIP()
);
#125=(
REPRESENTATION_RELATIONSHIP($,$,#15120,#15069)
REPRESENTATION_RELATIONSHIP_WITH_TRANSFORMATION(#46)
SHAPE_REPRESENTATION_RELATIONSHIP()
);
#126=(
REPRESENTATION_RELATIONSHIP($,$,#15120,#15069)
REPRESENTATION_RELATIONSHIP_WITH_TRANSFORMATION(#47)
SHAPE_REPRESENTATION_RELATIONSHIP()
);
#127=(
REPRESENTATION_RELATIONSHIP($,$,#15120,#15069)
REPRESENTATION_RELATIONSHIP_WITH_TRANSFORMATION(#48)
SHAPE_REPRESENTATION_RELATIONSHIP()
);
#128=(
REPRESENTATION_RELATIONSHIP($,$,#15120,#15069)
REPRESENTATION_RELATIONSHIP_WITH_TRANSFORMATION(#49)
SHAPE_REPRESENTATION_RELATIONSHIP()
);
#129=(
REPRESENTATION_RELATIONSHIP($,$,#15119,#15069)
REPRESENTATION_RELATIONSHIP_WITH_TRANSFORMATION(#50)
SHAPE_REPRESENTATION_RELATIONSHIP()
);
#130=(
REPRESENTATION_RELATIONSHIP($,$,#15119,#15069)
REPRESENTATION_RELATIONSHIP_WITH_TRANSFORMATION(#51)
SHAPE_REPRESENTATION_RELATIONSHIP()
);
#131=(
REPRESENTATION_RELATIONSHIP($,$,#15119,#15069)
REPRESENTATION_RELATIONSHIP_WITH_TRANSFORMATION(#52)
SHAPE_REPRESENTATION_RELATIONSHIP()
);
#132=(
REPRESENTATION_RELATIONSHIP($,$,#15119,#15069)
REPRESENTATION_RELATIONSHIP_WITH_TRANSFORMATION(#53)
SHAPE_REPRESENTATION_RELATIONSHIP()
);
#133=(
REPRESENTATION_RELATIONSHIP($,$,#15078,#15069)
REPRESENTATION_RELATIONSHIP_WITH_TRANSFORMATION(#54)
SHAPE_REPRESENTATION_RELATIONSHIP()
);
#134=(
REPRESENTATION_RELATIONSHIP($,$,#15120,#15069)
REPRESENTATION_RELATIONSHIP_WITH_TRANSFORMATION(#55)
SHAPE_REPRESENTATION_RELATIONSHIP()
);
#135=(
REPRESENTATION_RELATIONSHIP($,$,#15120,#15069)
REPRESENTATION_RELATIONSHIP_WITH_TRANSFORMATION(#56)
SHAPE_REPRESENTATION_RELATIONSHIP()
);
#136=(
REPRESENTATION_RELATIONSHIP($,$,#15120,#15069)
REPRESENTATION_RELATIONSHIP_WITH_TRANSFORMATION(#57)
SHAPE_REPRESENTATION_RELATIONSHIP()
);
#137=(
REPRESENTATION_RELATIONSHIP($,$,#15120,#15069)
REPRESENTATION_RELATIONSHIP_WITH_TRANSFORMATION(#58)
SHAPE_REPRESENTATION_RELATIONSHIP()
);
#138=(
REPRESENTATION_RELATIONSHIP($,$,#15085,#15084)
REPRESENTATION_RELATIONSHIP_WITH_TRANSFORMATION(#59)
SHAPE_REPRESENTATION_RELATIONSHIP()
);
#139=(
REPRESENTATION_RELATIONSHIP($,$,#15086,#15084)
REPRESENTATION_RELATIONSHIP_WITH_TRANSFORMATION(#60)
SHAPE_REPRESENTATION_RELATIONSHIP()
);
#140=(
REPRESENTATION_RELATIONSHIP($,$,#15087,#15084)
REPRESENTATION_RELATIONSHIP_WITH_TRANSFORMATION(#61)
SHAPE_REPRESENTATION_RELATIONSHIP()
);
#141=(
REPRESENTATION_RELATIONSHIP($,$,#15088,#15084)
REPRESENTATION_RELATIONSHIP_WITH_TRANSFORMATION(#62)
SHAPE_REPRESENTATION_RELATIONSHIP()
);
#142=(
REPRESENTATION_RELATIONSHIP($,$,#15089,#15084)
REPRESENTATION_RELATIONSHIP_WITH_TRANSFORMATION(#63)
SHAPE_REPRESENTATION_RELATIONSHIP()
);
#143=(
REPRESENTATION_RELATIONSHIP($,$,#15090,#15084)
REPRESENTATION_RELATIONSHIP_WITH_TRANSFORMATION(#64)
SHAPE_REPRESENTATION_RELATIONSHIP()
);
#144=(
REPRESENTATION_RELATIONSHIP($,$,#15091,#15084)
REPRESENTATION_RELATIONSHIP_WITH_TRANSFORMATION(#65)
SHAPE_REPRESENTATION_RELATIONSHIP()
);
#145=(
REPRESENTATION_RELATIONSHIP($,$,#15092,#15084)
REPRESENTATION_RELATIONSHIP_WITH_TRANSFORMATION(#66)
SHAPE_REPRESENTATION_RELATIONSHIP()
);
#146=(
REPRESENTATION_RELATIONSHIP($,$,#15093,#15084)
REPRESENTATION_RELATIONSHIP_WITH_TRANSFORMATION(#67)
SHAPE_REPRESENTATION_RELATIONSHIP()
);
#147=(
REPRESENTATION_RELATIONSHIP($,$,#15102,#15084)
REPRESENTATION_RELATIONSHIP_WITH_TRANSFORMATION(#68)
SHAPE_REPRESENTATION_RELATIONSHIP()
);
#148=(
REPRESENTATION_RELATIONSHIP($,$,#15120,#15084)
REPRESENTATION_RELATIONSHIP_WITH_TRANSFORMATION(#69)
SHAPE_REPRESENTATION_RELATIONSHIP()
);
#149=(
REPRESENTATION_RELATIONSHIP($,$,#15095,#15094)
REPRESENTATION_RELATIONSHIP_WITH_TRANSFORMATION(#70)
SHAPE_REPRESENTATION_RELATIONSHIP()
);
#150=(
REPRESENTATION_RELATIONSHIP($,$,#15096,#15094)
REPRESENTATION_RELATIONSHIP_WITH_TRANSFORMATION(#71)
SHAPE_REPRESENTATION_RELATIONSHIP()
);
#151=(
REPRESENTATION_RELATIONSHIP($,$,#15097,#15094)
REPRESENTATION_RELATIONSHIP_WITH_TRANSFORMATION(#72)
SHAPE_REPRESENTATION_RELATIONSHIP()
);
#152=(
REPRESENTATION_RELATIONSHIP($,$,#15098,#15094)
REPRESENTATION_RELATIONSHIP_WITH_TRANSFORMATION(#73)
SHAPE_REPRESENTATION_RELATIONSHIP()
);
#153=(
REPRESENTATION_RELATIONSHIP($,$,#15099,#15094)
REPRESENTATION_RELATIONSHIP_WITH_TRANSFORMATION(#74)
SHAPE_REPRESENTATION_RELATIONSHIP()
);
#154=(
REPRESENTATION_RELATIONSHIP($,$,#15100,#15094)
REPRESENTATION_RELATIONSHIP_WITH_TRANSFORMATION(#75)
SHAPE_REPRESENTATION_RELATIONSHIP()
);
#155=(
REPRESENTATION_RELATIONSHIP($,$,#15101,#15094)
REPRESENTATION_RELATIONSHIP_WITH_TRANSFORMATION(#76)
SHAPE_REPRESENTATION_RELATIONSHIP()
);
#156=(
REPRESENTATION_RELATIONSHIP($,$,#15102,#15094)
REPRESENTATION_RELATIONSHIP_WITH_TRANSFORMATION(#77)
SHAPE_REPRESENTATION_RELATIONSHIP()
);
#157=(
REPRESENTATION_RELATIONSHIP($,$,#15120,#15094)
REPRESENTATION_RELATIONSHIP_WITH_TRANSFORMATION(#78)
SHAPE_REPRESENTATION_RELATIONSHIP()
);
#158=(
REPRESENTATION_RELATIONSHIP($,$,#15110,#15109)
REPRESENTATION_RELATIONSHIP_WITH_TRANSFORMATION(#79)
SHAPE_REPRESENTATION_RELATIONSHIP()
);
#159=(
REPRESENTATION_RELATIONSHIP($,$,#15111,#15109)
REPRESENTATION_RELATIONSHIP_WITH_TRANSFORMATION(#80)
SHAPE_REPRESENTATION_RELATIONSHIP()
);
#160=(
REPRESENTATION_RELATIONSHIP($,$,#15112,#15109)
REPRESENTATION_RELATIONSHIP_WITH_TRANSFORMATION(#81)
SHAPE_REPRESENTATION_RELATIONSHIP()
);
#161=(
REPRESENTATION_RELATIONSHIP($,$,#15113,#15109)
REPRESENTATION_RELATIONSHIP_WITH_TRANSFORMATION(#82)
SHAPE_REPRESENTATION_RELATIONSHIP()
);
#162=(
REPRESENTATION_RELATIONSHIP($,$,#15114,#15109)
REPRESENTATION_RELATIONSHIP_WITH_TRANSFORMATION(#83)
SHAPE_REPRESENTATION_RELATIONSHIP()
);
#163=(
REPRESENTATION_RELATIONSHIP($,$,#15115,#15109)
REPRESENTATION_RELATIONSHIP_WITH_TRANSFORMATION(#84)
SHAPE_REPRESENTATION_RELATIONSHIP()
);
#164=(
REPRESENTATION_RELATIONSHIP($,$,#15119,#15109)
REPRESENTATION_RELATIONSHIP_WITH_TRANSFORMATION(#85)
SHAPE_REPRESENTATION_RELATIONSHIP()
);
#165=(
REPRESENTATION_RELATIONSHIP($,$,#15119,#15109)
REPRESENTATION_RELATIONSHIP_WITH_TRANSFORMATION(#86)
SHAPE_REPRESENTATION_RELATIONSHIP()
);
#166=(
REPRESENTATION_RELATIONSHIP($,$,#15119,#15109)
REPRESENTATION_RELATIONSHIP_WITH_TRANSFORMATION(#87)
SHAPE_REPRESENTATION_RELATIONSHIP()
);
#167=(
REPRESENTATION_RELATIONSHIP($,$,#15119,#15109)
REPRESENTATION_RELATIONSHIP_WITH_TRANSFORMATION(#88)
SHAPE_REPRESENTATION_RELATIONSHIP()
);
#168=(
REPRESENTATION_RELATIONSHIP($,$,#15120,#15109)
REPRESENTATION_RELATIONSHIP_WITH_TRANSFORMATION(#89)
SHAPE_REPRESENTATION_RELATIONSHIP()
);
#169=(
REPRESENTATION_RELATIONSHIP($,$,#15069,#15068)
REPRESENTATION_RELATIONSHIP_WITH_TRANSFORMATION(#90)
SHAPE_REPRESENTATION_RELATIONSHIP()
);
#170=(
REPRESENTATION_RELATIONSHIP($,$,#15084,#15068)
REPRESENTATION_RELATIONSHIP_WITH_TRANSFORMATION(#91)
SHAPE_REPRESENTATION_RELATIONSHIP()
);
#171=(
REPRESENTATION_RELATIONSHIP($,$,#15094,#15068)
REPRESENTATION_RELATIONSHIP_WITH_TRANSFORMATION(#92)
SHAPE_REPRESENTATION_RELATIONSHIP()
);
#172=(
REPRESENTATION_RELATIONSHIP($,$,#15103,#15068)
REPRESENTATION_RELATIONSHIP_WITH_TRANSFORMATION(#93)
SHAPE_REPRESENTATION_RELATIONSHIP()
);
#173=(
REPRESENTATION_RELATIONSHIP($,$,#15105,#15068)
REPRESENTATION_RELATIONSHIP_WITH_TRANSFORMATION(#94)
SHAPE_REPRESENTATION_RELATIONSHIP()
);
#174=(
REPRESENTATION_RELATIONSHIP($,$,#15109,#15068)
REPRESENTATION_RELATIONSHIP_WITH_TRANSFORMATION(#95)
SHAPE_REPRESENTATION_RELATIONSHIP()
);
#175=CONTEXT_DEPENDENT_SHAPE_REPRESENTATION(#96,#14952);
#176=CONTEXT_DEPENDENT_SHAPE_REPRESENTATION(#97,#14953);
#177=CONTEXT_DEPENDENT_SHAPE_REPRESENTATION(#98,#14954);
#178=CONTEXT_DEPENDENT_SHAPE_REPRESENTATION(#99,#14955);
#179=CONTEXT_DEPENDENT_SHAPE_REPRESENTATION(#100,#14956);
#180=CONTEXT_DEPENDENT_SHAPE_REPRESENTATION(#101,#14978);
#181=CONTEXT_DEPENDENT_SHAPE_REPRESENTATION(#102,#14983);
#182=CONTEXT_DEPENDENT_SHAPE_REPRESENTATION(#103,#14984);
#183=CONTEXT_DEPENDENT_SHAPE_REPRESENTATION(#104,#14985);
#184=CONTEXT_DEPENDENT_SHAPE_REPRESENTATION(#105,#14996);
#185=CONTEXT_DEPENDENT_SHAPE_REPRESENTATION(#106,#14997);
#186=CONTEXT_DEPENDENT_SHAPE_REPRESENTATION(#107,#14998);
#187=CONTEXT_DEPENDENT_SHAPE_REPRESENTATION(#108,#15001);
#188=CONTEXT_DEPENDENT_SHAPE_REPRESENTATION(#109,#15002);
#189=CONTEXT_DEPENDENT_SHAPE_REPRESENTATION(#110,#15003);
#190=CONTEXT_DEPENDENT_SHAPE_REPRESENTATION(#111,#15004);
#191=CONTEXT_DEPENDENT_SHAPE_REPRESENTATION(#112,#15005);
#192=CONTEXT_DEPENDENT_SHAPE_REPRESENTATION(#113,#15006);
#193=CONTEXT_DEPENDENT_SHAPE_REPRESENTATION(#114,#15007);
#194=CONTEXT_DEPENDENT_SHAPE_REPRESENTATION(#115,#15008);
#195=CONTEXT_DEPENDENT_SHAPE_REPRESENTATION(#116,#15009);
#196=CONTEXT_DEPENDENT_SHAPE_REPRESENTATION(#117,#15010);
#197=CONTEXT_DEPENDENT_SHAPE_REPRESENTATION(#118,#15011);
#198=CONTEXT_DEPENDENT_SHAPE_REPRESENTATION(#119,#15012);
#199=CONTEXT_DEPENDENT_SHAPE_REPRESENTATION(#120,#15013);
#200=CONTEXT_DEPENDENT_SHAPE_REPRESENTATION(#121,#15014);
#201=CONTEXT_DEPENDENT_SHAPE_REPRESENTATION(#122,#15015);
#202=CONTEXT_DEPENDENT_SHAPE_REPRESENTATION(#123,#15016);
#203=CONTEXT_DEPENDENT_SHAPE_REPRESENTATION(#124,#15017);
#204=CONTEXT_DEPENDENT_SHAPE_REPRESENTATION(#125,#15018);
#205=CONTEXT_DEPENDENT_SHAPE_REPRESENTATION(#126,#15019);
#206=CONTEXT_DEPENDENT_SHAPE_REPRESENTATION(#127,#15020);
#207=CONTEXT_DEPENDENT_SHAPE_REPRESENTATION(#128,#15021);
#208=CONTEXT_DEPENDENT_SHAPE_REPRESENTATION(#129,#15022);
#209=CONTEXT_DEPENDENT_SHAPE_REPRESENTATION(#130,#15023);
#210=CONTEXT_DEPENDENT_SHAPE_REPRESENTATION(#131,#15024);
#211=CONTEXT_DEPENDENT_SHAPE_REPRESENTATION(#132,#15025);
#212=CONTEXT_DEPENDENT_SHAPE_REPRESENTATION(#133,#15026);
#213=CONTEXT_DEPENDENT_SHAPE_REPRESENTATION(#134,#15027);
#214=CONTEXT_DEPENDENT_SHAPE_REPRESENTATION(#135,#15028);
#215=CONTEXT_DEPENDENT_SHAPE_REPRESENTATION(#136,#15029);
#216=CONTEXT_DEPENDENT_SHAPE_REPRESENTATION(#137,#15030);
#217=CONTEXT_DEPENDENT_SHAPE_REPRESENTATION(#138,#15031);
#218=CONTEXT_DEPENDENT_SHAPE_REPRESENTATION(#139,#15032);
#219=CONTEXT_DEPENDENT_SHAPE_REPRESENTATION(#140,#15033);
#220=CONTEXT_DEPENDENT_SHAPE_REPRESENTATION(#141,#15034);
#221=CONTEXT_DEPENDENT_SHAPE_REPRESENTATION(#142,#15035);
#222=CONTEXT_DEPENDENT_SHAPE_REPRESENTATION(#143,#15036);
#223=CONTEXT_DEPENDENT_SHAPE_REPRESENTATION(#144,#15037);
#224=CONTEXT_DEPENDENT_SHAPE_REPRESENTATION(#145,#15038);
#225=CONTEXT_DEPENDENT_SHAPE_REPRESENTATION(#146,#15039);
#226=CONTEXT_DEPENDENT_SHAPE_REPRESENTATION(#147,#15040);
#227=CONTEXT_DEPENDENT_SHAPE_REPRESENTATION(#148,#15041);
#228=CONTEXT_DEPENDENT_SHAPE_REPRESENTATION(#149,#15042);
#229=CONTEXT_DEPENDENT_SHAPE_REPRESENTATION(#150,#15043);
#230=CONTEXT_DEPENDENT_SHAPE_REPRESENTATION(#151,#15044);
#231=CONTEXT_DEPENDENT_SHAPE_REPRESENTATION(#152,#15045);
#232=CONTEXT_DEPENDENT_SHAPE_REPRESENTATION(#153,#15046);
#233=CONTEXT_DEPENDENT_SHAPE_REPRESENTATION(#154,#15047);
#234=CONTEXT_DEPENDENT_SHAPE_REPRESENTATION(#155,#15048);
#235=CONTEXT_DEPENDENT_SHAPE_REPRESENTATION(#156,#15049);
#236=CONTEXT_DEPENDENT_SHAPE_REPRESENTATION(#157,#15050);
#237=CONTEXT_DEPENDENT_SHAPE_REPRESENTATION(#158,#15051);
#238=CONTEXT_DEPENDENT_SHAPE_REPRESENTATION(#159,#15052);
#239=CONTEXT_DEPENDENT_SHAPE_REPRESENTATION(#160,#15053);
#240=CONTEXT_DEPENDENT_SHAPE_REPRESENTATION(#161,#15054);
#241=CONTEXT_DEPENDENT_SHAPE_REPRESENTATION(#162,#15055);
#242=CONTEXT_DEPENDENT_SHAPE_REPRESENTATION(#163,#15056);
#243=CONTEXT_DEPENDENT_SHAPE_REPRESENTATION(#164,#15057);
#244=CONTEXT_DEPENDENT_SHAPE_REPRESENTATION(#165,#15058);
#245=CONTEXT_DEPENDENT_SHAPE_REPRESENTATION(#166,#15059);
#246=CONTEXT_DEPENDENT_SHAPE_REPRESENTATION(#167,#15060);
#247=CONTEXT_DEPENDENT_SHAPE_REPRESENTATION(#168,#15061);
#248=CONTEXT_DEPENDENT_SHAPE_REPRESENTATION(#169,#15062);
#249=CONTEXT_DEPENDENT_SHAPE_REPRESENTATION(#170,#15063);
#250=CONTEXT_DEPENDENT_SHAPE_REPRESENTATION(#171,#15064);
#251=CONTEXT_DEPENDENT_SHAPE_REPRESENTATION(#172,#15065);
#252=CONTEXT_DEPENDENT_SHAPE_REPRESENTATION(#173,#15066);
#253=CONTEXT_DEPENDENT_SHAPE_REPRESENTATION(#174,#15067);
#254=NEXT_ASSEMBLY_USAGE_OCCURRENCE('Inner ring:1','Inner ring:1',
'Inner ring:1',#15132,#15133,'Inner ring:1');
#255=NEXT_ASSEMBLY_USAGE_OCCURRENCE('Outer ring:1','Outer ring:1',
'Outer ring:1',#15132,#15134,'Outer ring:1');
#256=NEXT_ASSEMBLY_USAGE_OCCURRENCE('Balls:1','Balls:1','Balls:1',#15132,
#15135,'Balls:1');
#257=NEXT_ASSEMBLY_USAGE_OCCURRENCE('Cage:1','Cage:1','Cage:1',#15132,#15136,
'Cage:1');
#258=NEXT_ASSEMBLY_USAGE_OCCURRENCE('Seals 2RS:1','Seals 2RS:1',
'Seals 2RS:1',#15132,#15137,'Seals 2RS:1');
#259=NEXT_ASSEMBLY_USAGE_OCCURRENCE('Captive sliding block:1',
'Captive sliding block:1','Captive sliding block:1',#15157,#15158,
'Captive sliding block:1');
#260=NEXT_ASSEMBLY_USAGE_OCCURRENCE('Connecting link:1',
'Connecting link:1','Connecting link:1',#15159,#15160,
'Connecting link:1');
#261=NEXT_ASSEMBLY_USAGE_OCCURRENCE('Link bushing:1','Link bushing:1',
'Link bushing:1',#15159,#15161,'Link bushing:1');
#262=NEXT_ASSEMBLY_USAGE_OCCURRENCE('Link bushing (1):1',
'Link bushing (1):1','Link bushing (1):1',#15159,#15162,
'Link bushing (1):1');
#263=NEXT_ASSEMBLY_USAGE_OCCURRENCE('Block:1','Block:1','Block:1',#15169,
#15170,'Block:1');
#264=NEXT_ASSEMBLY_USAGE_OCCURRENCE('End cap +:1','End cap +:1',
'End cap +:1',#15169,#15171,'End cap +:1');
#265=NEXT_ASSEMBLY_USAGE_OCCURRENCE('End cap:1','End cap:1','End cap:1',
#15169,#15172,'End cap:1');
#266=NEXT_ASSEMBLY_USAGE_OCCURRENCE('Base:1','Base:1','Base:1',#15123,#15124,
'Base:1');
#267=NEXT_ASSEMBLY_USAGE_OCCURRENCE('Foot strip:1','Foot strip:1',
'Foot strip:1',#15123,#15125,'Foot strip:1');
#268=NEXT_ASSEMBLY_USAGE_OCCURRENCE('Foot strip (1):1',
'Foot strip (1):1','Foot strip (1):1',#15123,#15126,'Foot strip (1):1');
#269=NEXT_ASSEMBLY_USAGE_OCCURRENCE('Lever bearing post:1',
'Lever bearing post:1','Lever bearing post:1',#15123,#15127,
'Lever bearing post:1');
#270=NEXT_ASSEMBLY_USAGE_OCCURRENCE('Bearing cap:1','Bearing cap:1',
'Bearing cap:1',#15123,#15128,'Bearing cap:1');
#271=NEXT_ASSEMBLY_USAGE_OCCURRENCE('Crank bearing post:1',
'Crank bearing post:1','Crank bearing post:1',#15123,#15129,
'Crank bearing post:1');
#272=NEXT_ASSEMBLY_USAGE_OCCURRENCE('Bearing cap (1):1',
'Bearing cap (1):1','Bearing cap (1):1',#15123,#15130,
'Bearing cap (1):1');
#273=NEXT_ASSEMBLY_USAGE_OCCURRENCE(
'Linear Guide Rail - 15 mm, 220 mm Long:2',
'Linear Guide Rail - 15 mm, 220 mm Long:2',
'Linear Guide Rail - 15 mm, 220 mm Long:2',#15123,#15131,
'Linear Guide Rail - 15 mm, 220 mm Long:2');
#274=NEXT_ASSEMBLY_USAGE_OCCURRENCE('Cap Screw - M4x16:2',
'Cap Screw - M4x16:2','Cap Screw - M4x16:2',#15123,#15147,
'Cap Screw - M4x16:2');
#275=NEXT_ASSEMBLY_USAGE_OCCURRENCE('Cap Screw - M4x16:3',
'Cap Screw - M4x16:3','Cap Screw - M4x16:3',#15123,#15147,
'Cap Screw - M4x16:3');
#276=NEXT_ASSEMBLY_USAGE_OCCURRENCE('Cap Screw - M4x16:4',
'Cap Screw - M4x16:4','Cap Screw - M4x16:4',#15123,#15147,
'Cap Screw - M4x16:4');
#277=NEXT_ASSEMBLY_USAGE_OCCURRENCE('Cap Screw - M4x16:5',
'Cap Screw - M4x16:5','Cap Screw - M4x16:5',#15123,#15147,
'Cap Screw - M4x16:5');
#278=NEXT_ASSEMBLY_USAGE_OCCURRENCE('M5x14 Cap Screw:6',
'M5x14 Cap Screw:6','M5x14 Cap Screw:6',#15123,#15173,
'M5x14 Cap Screw:6');
#279=NEXT_ASSEMBLY_USAGE_OCCURRENCE('M5x14 Cap Screw:7',
'M5x14 Cap Screw:7','M5x14 Cap Screw:7',#15123,#15173,
'M5x14 Cap Screw:7');
#280=NEXT_ASSEMBLY_USAGE_OCCURRENCE('M5x14 Cap Screw:8',
'M5x14 Cap Screw:8','M5x14 Cap Screw:8',#15123,#15173,
'M5x14 Cap Screw:8');
#281=NEXT_ASSEMBLY_USAGE_OCCURRENCE('M5x14 Cap Screw:9',
'M5x14 Cap Screw:9','M5x14 Cap Screw:9',#15123,#15173,
'M5x14 Cap Screw:9');
#282=NEXT_ASSEMBLY_USAGE_OCCURRENCE(
'Sealed Ball Bearing - 10 x 30 x 9 mm:2',
'Sealed Ball Bearing - 10 x 30 x 9 mm:2',
'Sealed Ball Bearing - 10 x 30 x 9 mm:2',#15123,#15132,
'Sealed Ball Bearing - 10 x 30 x 9 mm:2');
#283=NEXT_ASSEMBLY_USAGE_OCCURRENCE('M4x10 Cap Screw:2',
'M4x10 Cap Screw:2','M4x10 Cap Screw:2',#15123,#15174,
'M4x10 Cap Screw:2');
#284=NEXT_ASSEMBLY_USAGE_OCCURRENCE('M4x10 Cap Screw:3',
'M4x10 Cap Screw:3','M4x10 Cap Screw:3',#15123,#15174,
'M4x10 Cap Screw:3');
#285=NEXT_ASSEMBLY_USAGE_OCCURRENCE('M4x10 Cap Screw:4',
'M4x10 Cap Screw:4','M4x10 Cap Screw:4',#15123,#15174,
'M4x10 Cap Screw:4');
#286=NEXT_ASSEMBLY_USAGE_OCCURRENCE('M4x10 Cap Screw:5',
'M4x10 Cap Screw:5','M4x10 Cap Screw:5',#15123,#15174,
'M4x10 Cap Screw:5');
#287=NEXT_ASSEMBLY_USAGE_OCCURRENCE('M5x14 Cap Screw:10',
'M5x14 Cap Screw:10','M5x14 Cap Screw:10',#15123,#15173,
'M5x14 Cap Screw:10');
#288=NEXT_ASSEMBLY_USAGE_OCCURRENCE('M5x14 Cap Screw:11',
'M5x14 Cap Screw:11','M5x14 Cap Screw:11',#15123,#15173,
'M5x14 Cap Screw:11');
#289=NEXT_ASSEMBLY_USAGE_OCCURRENCE('M5x14 Cap Screw:12',
'M5x14 Cap Screw:12','M5x14 Cap Screw:12',#15123,#15173,
'M5x14 Cap Screw:12');
#290=NEXT_ASSEMBLY_USAGE_OCCURRENCE('M5x14 Cap Screw:13',
'M5x14 Cap Screw:13','M5x14 Cap Screw:13',#15123,#15173,
'M5x14 Cap Screw:13');
#291=NEXT_ASSEMBLY_USAGE_OCCURRENCE(
'Sealed Ball Bearing - 10 x 30 x 9 mm:3',
'Sealed Ball Bearing - 10 x 30 x 9 mm:3',
'Sealed Ball Bearing - 10 x 30 x 9 mm:3',#15123,#15132,
'Sealed Ball Bearing - 10 x 30 x 9 mm:3');
#292=NEXT_ASSEMBLY_USAGE_OCCURRENCE('M4x10 Cap Screw:6',
'M4x10 Cap Screw:6','M4x10 Cap Screw:6',#15123,#15174,
'M4x10 Cap Screw:6');
#293=NEXT_ASSEMBLY_USAGE_OCCURRENCE('M4x10 Cap Screw:7',
'M4x10 Cap Screw:7','M4x10 Cap Screw:7',#15123,#15174,
'M4x10 Cap Screw:7');
#294=NEXT_ASSEMBLY_USAGE_OCCURRENCE('M4x10 Cap Screw:8',
'M4x10 Cap Screw:8','M4x10 Cap Screw:8',#15123,#15174,
'M4x10 Cap Screw:8');
#295=NEXT_ASSEMBLY_USAGE_OCCURRENCE('M4x10 Cap Screw:9',
'M4x10 Cap Screw:9','M4x10 Cap Screw:9',#15123,#15174,
'M4x10 Cap Screw:9');
#296=NEXT_ASSEMBLY_USAGE_OCCURRENCE('Input crank and spindle:1',
'Input crank and spindle:1','Input crank and spindle:1',#15138,#15139,
'Input crank and spindle:1');
#297=NEXT_ASSEMBLY_USAGE_OCCURRENCE('Underside input grip:1',
'Underside input grip:1','Underside input grip:1',#15138,#15140,
'Underside input grip:1');
#298=NEXT_ASSEMBLY_USAGE_OCCURRENCE('Lower bearing sleeve:1',
'Lower bearing sleeve:1','Lower bearing sleeve:1',#15138,#15141,
'Lower bearing sleeve:1');
#299=NEXT_ASSEMBLY_USAGE_OCCURRENCE('Shaft collar:1','Shaft collar:1',
'Shaft collar:1',#15138,#15142,'Shaft collar:1');
#300=NEXT_ASSEMBLY_USAGE_OCCURRENCE('Crank pin:1','Crank pin:1',
'Crank pin:1',#15138,#15143,'Crank pin:1');
#301=NEXT_ASSEMBLY_USAGE_OCCURRENCE('Crank lower spacer:1',
'Crank lower spacer:1','Crank lower spacer:1',#15138,#15144,
'Crank lower spacer:1');
#302=NEXT_ASSEMBLY_USAGE_OCCURRENCE('Pin upper spacer:1',
'Pin upper spacer:1','Pin upper spacer:1',#15138,#15145,
'Pin upper spacer:1');
#303=NEXT_ASSEMBLY_USAGE_OCCURRENCE('Pin keeper:1','Pin keeper:1',
'Pin keeper:1',#15138,#15146,'Pin keeper:1');
#304=NEXT_ASSEMBLY_USAGE_OCCURRENCE('Cap Screw - M4x16:6',
'Cap Screw - M4x16:6','Cap Screw - M4x16:6',#15138,#15147,
'Cap Screw - M4x16:6');
#305=NEXT_ASSEMBLY_USAGE_OCCURRENCE('M4x4 collar screw:3',
'M4x4 collar screw:3','M4x4 collar screw:3',#15138,#15156,
'M4x4 collar screw:3');
#306=NEXT_ASSEMBLY_USAGE_OCCURRENCE('M4x10 Cap Screw:10',
'M4x10 Cap Screw:10','M4x10 Cap Screw:10',#15138,#15174,
'M4x10 Cap Screw:10');
#307=NEXT_ASSEMBLY_USAGE_OCCURRENCE('Slotted lever and spindle:1',
'Slotted lever and spindle:1','Slotted lever and spindle:1',#15148,#15149,
'Slotted lever and spindle:1');
#308=NEXT_ASSEMBLY_USAGE_OCCURRENCE('Lower bearing sleeve (1):1',
'Lower bearing sleeve (1):1','Lower bearing sleeve (1):1',#15148,#15150,
'Lower bearing sleeve (1):1');
#309=NEXT_ASSEMBLY_USAGE_OCCURRENCE('Shaft collar (1):1',
'Shaft collar (1):1','Shaft collar (1):1',#15148,#15151,
'Shaft collar (1):1');
#310=NEXT_ASSEMBLY_USAGE_OCCURRENCE('Lever output pin:1',
'Lever output pin:1','Lever output pin:1',#15148,#15152,
'Lever output pin:1');
#311=NEXT_ASSEMBLY_USAGE_OCCURRENCE('Lever output lower spacer:1',
'Lever output lower spacer:1','Lever output lower spacer:1',#15148,#15153,
'Lever output lower spacer:1');
#312=NEXT_ASSEMBLY_USAGE_OCCURRENCE('Pin upper spacer (1):1',
'Pin upper spacer (1):1','Pin upper spacer (1):1',#15148,#15154,
'Pin upper spacer (1):1');
#313=NEXT_ASSEMBLY_USAGE_OCCURRENCE('Pin keeper (1):1',
'Pin keeper (1):1','Pin keeper (1):1',#15148,#15155,'Pin keeper (1):1');
#314=NEXT_ASSEMBLY_USAGE_OCCURRENCE('M4x4 collar screw:2',
'M4x4 collar screw:2','M4x4 collar screw:2',#15148,#15156,
'M4x4 collar screw:2');
#315=NEXT_ASSEMBLY_USAGE_OCCURRENCE('M4x10 Cap Screw:11',
'M4x10 Cap Screw:11','M4x10 Cap Screw:11',#15148,#15174,
'M4x10 Cap Screw:11');
#316=NEXT_ASSEMBLY_USAGE_OCCURRENCE('Ram table:1','Ram table:1',
'Ram table:1',#15163,#15164,'Ram table:1');
#317=NEXT_ASSEMBLY_USAGE_OCCURRENCE('Ram pin:1','Ram pin:1','Ram pin:1',
#15163,#15165,'Ram pin:1');
#318=NEXT_ASSEMBLY_USAGE_OCCURRENCE('Ram lower spacer:1',
'Ram lower spacer:1','Ram lower spacer:1',#15163,#15166,
'Ram lower spacer:1');
#319=NEXT_ASSEMBLY_USAGE_OCCURRENCE('Pin upper spacer (2):1',
'Pin upper spacer (2):1','Pin upper spacer (2):1',#15163,#15167,
'Pin upper spacer (2):1');
#320=NEXT_ASSEMBLY_USAGE_OCCURRENCE('Pin keeper (2):1',
'Pin keeper (2):1','Pin keeper (2):1',#15163,#15168,'Pin keeper (2):1');
#321=NEXT_ASSEMBLY_USAGE_OCCURRENCE(
'Flanged Linear Guide Carriage - 15 mm:2',
'Flanged Linear Guide Carriage - 15 mm:2',
'Flanged Linear Guide Carriage - 15 mm:2',#15163,#15169,
'Flanged Linear Guide Carriage - 15 mm:2');
#322=NEXT_ASSEMBLY_USAGE_OCCURRENCE('M5x14 Cap Screw:2',
'M5x14 Cap Screw:2','M5x14 Cap Screw:2',#15163,#15173,
'M5x14 Cap Screw:2');
#323=NEXT_ASSEMBLY_USAGE_OCCURRENCE('M5x14 Cap Screw:3',
'M5x14 Cap Screw:3','M5x14 Cap Screw:3',#15163,#15173,
'M5x14 Cap Screw:3');
#324=NEXT_ASSEMBLY_USAGE_OCCURRENCE('M5x14 Cap Screw:4',
'M5x14 Cap Screw:4','M5x14 Cap Screw:4',#15163,#15173,
'M5x14 Cap Screw:4');
#325=NEXT_ASSEMBLY_USAGE_OCCURRENCE('M5x14 Cap Screw:5',
'M5x14 Cap Screw:5','M5x14 Cap Screw:5',#15163,#15173,
'M5x14 Cap Screw:5');
#326=NEXT_ASSEMBLY_USAGE_OCCURRENCE('M4x10 Cap Screw:12',
'M4x10 Cap Screw:12','M4x10 Cap Screw:12',#15163,#15174,
'M4x10 Cap Screw:12');
#327=NEXT_ASSEMBLY_USAGE_OCCURRENCE('Bearing base and output rail:1',
'Bearing base and output rail:1','Bearing base and output rail:1',#15122,
#15123,'Bearing base and output rail:1');
#328=NEXT_ASSEMBLY_USAGE_OCCURRENCE('Driving crank:1','Driving crank:1',
'Driving crank:1',#15122,#15138,'Driving crank:1');
#329=NEXT_ASSEMBLY_USAGE_OCCURRENCE('Slotted lever:1','Slotted lever:1',
'Slotted lever:1',#15122,#15148,'Slotted lever:1');
#330=NEXT_ASSEMBLY_USAGE_OCCURRENCE('Sliding crank block:1',
'Sliding crank block:1','Sliding crank block:1',#15122,#15157,
'Sliding crank block:1');
#331=NEXT_ASSEMBLY_USAGE_OCCURRENCE('Output link:1','Output link:1',
'Output link:1',#15122,#15159,'Output link:1');
#332=NEXT_ASSEMBLY_USAGE_OCCURRENCE('Guided output ram:1',
'Guided output ram:1','Guided output ram:1',#15122,#15163,
'Guided output ram:1');
#333=SPHERICAL_SURFACE('',#8750,0.23815);
#334=SPHERICAL_SURFACE('',#8752,0.23815);
#335=SPHERICAL_SURFACE('',#8754,0.23815);
#336=SPHERICAL_SURFACE('',#8756,0.23815);
#337=SPHERICAL_SURFACE('',#8758,0.23815);
#338=SPHERICAL_SURFACE('',#8760,0.23815);
#339=SPHERICAL_SURFACE('',#8762,0.23815);
#340=SPHERICAL_SURFACE('',#8764,0.23815);
#341=SPHERICAL_SURFACE('',#8767,0.247676);
#342=SPHERICAL_SURFACE('',#8783,0.247676);
#343=SPHERICAL_SURFACE('',#8788,0.247676);
#344=SPHERICAL_SURFACE('',#8793,0.247676);
#345=SPHERICAL_SURFACE('',#8798,0.247676);
#346=SPHERICAL_SURFACE('',#8803,0.247676);
#347=SPHERICAL_SURFACE('',#8808,0.247676);
#348=SPHERICAL_SURFACE('',#8816,0.247676);
#349=CONICAL_SURFACE('',#8721,0.53,0.785398163397448);
#350=CONICAL_SURFACE('',#8728,0.53,0.785398163397448);
#351=CONICAL_SURFACE('',#8741,1.47,0.785398163397449);
#352=CONICAL_SURFACE('',#8745,1.47,0.785398163397449);
#353=CONICAL_SURFACE('',#8957,0.325,0.785398163397448);
#354=CONICAL_SURFACE('',#8961,0.335,0.785398163397448);
#355=CONICAL_SURFACE('',#8965,0.21,0.463647609000806);
#356=CONICAL_SURFACE('',#8969,0.18,0.785398163397448);
#357=CONICAL_SURFACE('',#9087,0.185,0.785398163397449);
#358=CONICAL_SURFACE('',#9295,0.4,0.785398163397448);
#359=CONICAL_SURFACE('',#9299,0.41,0.785398163397448);
#360=CONICAL_SURFACE('',#9303,0.26,0.463647609000806);
#361=CONICAL_SURFACE('',#9319,0.325,0.785398163397448);
#362=CONICAL_SURFACE('',#9323,0.335,0.785398163397448);
#363=CONICAL_SURFACE('',#9327,0.21,0.463647609000806);
#364=TOROIDAL_SURFACE('',#8710,1.,0.247676);
#365=TOROIDAL_SURFACE('',#8730,1.,0.247676);
#366=B_SPLINE_CURVE_WITH_KNOTS('',3,(#12105,#12106,#12107,#12108,#12109,
#12110,#12111,#12112,#12113,#12114),.UNSPECIFIED.,.F.,.F.,(4,2,2,2,4),(0.,
0.0945941824764479,0.189188364952896,0.283770357603024,0.378352350253152),
 .UNSPECIFIED.);
#367=B_SPLINE_CURVE_WITH_KNOTS('',3,(#12115,#12116,#12117,#12118,#12119,
#12120,#12121,#12122,#12123,#12124,#12125,#12126,#12127,#12128,#12129,#12130,
#12131,#12132,#12133,#12134,#12135,#12136,#12137,#12138,#12139,#12140),
 .UNSPECIFIED.,.F.,.F.,(4,2,2,2,2,2,2,2,2,2,2,2,4),(0.378352350253152,0.47293434290328,
0.567516335553408,0.662110518029855,0.756704700506303,0.851298882982751,
0.945893065459199,1.04047505810933,1.13505705075946,1.22963904340958,1.32422103605971,
1.41881521853616,1.51340940101261),.UNSPECIFIED.);
#368=B_SPLINE_CURVE_WITH_KNOTS('',3,(#12144,#12145,#12146,#12147,#12148,
#12149,#12150,#12151,#12152,#12153,#12154,#12155,#12156,#12157,#12158,#12159,
#12160,#12161,#12162,#12163,#12164,#12165,#12166,#12167,#12168,#12169),
 .UNSPECIFIED.,.F.,.F.,(4,2,2,2,2,2,2,2,2,2,2,2,4),(0.,0.0942219535700049,
0.18844390714001,0.282665684012033,0.376887460884057,0.471109237756081,
0.565331014628104,0.659552968198109,0.753774921768114,0.847996875338119,
0.942218828908124,1.03644060578015,1.13066238265217),.UNSPECIFIED.);
#369=B_SPLINE_CURVE_WITH_KNOTS('',3,(#12170,#12171,#12172,#12173,#12174,
#12175,#12176,#12177,#12178,#12179),.UNSPECIFIED.,.F.,.F.,(4,2,2,2,4),(1.13066238265217,
1.22488415952419,1.31910593639622,1.41332788996622,1.50754984353623),
 .UNSPECIFIED.);
#370=B_SPLINE_CURVE_WITH_KNOTS('',3,(#12386,#12387,#12388,#12389,#12390,
#12391,#12392,#12393,#12394,#12395),.UNSPECIFIED.,.F.,.F.,(4,2,2,2,4),(0.,
0.094594182476448,0.189188364952896,0.283770357603024,0.378352350253152),
 .UNSPECIFIED.);
#371=B_SPLINE_CURVE_WITH_KNOTS('',3,(#12396,#12397,#12398,#12399,#12400,
#12401,#12402,#12403,#12404,#12405,#12406,#12407,#12408,#12409,#12410,#12411,
#12412,#12413,#12414,#12415,#12416,#12417,#12418,#12419,#12420,#12421),
 .UNSPECIFIED.,.F.,.F.,(4,2,2,2,2,2,2,2,2,2,2,2,4),(0.378352350253152,0.472934342903279,
0.567516335553407,0.662110518029855,0.756704700506303,0.851298882982751,
0.945893065459199,1.04047505810933,1.13505705075945,1.22963904340958,1.32422103605971,
1.41881521853616,1.51340940101261),.UNSPECIFIED.);
#372=B_SPLINE_CURVE_WITH_KNOTS('',3,(#12425,#12426,#12427,#12428,#12429,
#12430,#12431,#12432,#12433,#12434,#12435,#12436,#12437,#12438,#12439,#12440,
#12441,#12442,#12443,#12444,#12445,#12446,#12447,#12448,#12449,#12450),
 .UNSPECIFIED.,.F.,.F.,(4,2,2,2,2,2,2,2,2,2,2,2,4),(0.,0.094221953570005,
0.18844390714001,0.282665684012033,0.376887460884057,0.47110923775608,0.565331014628104,
0.659552968198109,0.753774921768114,0.847996875338119,0.942218828908123,
1.03644060578015,1.13066238265217),.UNSPECIFIED.);
#373=B_SPLINE_CURVE_WITH_KNOTS('',3,(#12451,#12452,#12453,#12454,#12455,
#12456,#12457,#12458,#12459,#12460),.UNSPECIFIED.,.F.,.F.,(4,2,2,2,4),(1.13066238265217,
1.22488415952419,1.31910593639622,1.41332788996622,1.50754984353623),
 .UNSPECIFIED.);
#374=B_SPLINE_CURVE_WITH_KNOTS('',3,(#12898,#12899,#12900,#12901,#12902,
#12903,#12904,#12905,#12906,#12907,#12908,#12909,#12910,#12911,#12912,#12913,
#12914,#12915,#12916,#12917,#12918,#12919),.UNSPECIFIED.,.F.,.F.,(4,2,2,
2,2,2,2,2,2,2,4),(0.0473477652366656,0.126350602536658,0.189525903804987,
0.252701205073317,0.313298422430275,0.373895639787233,0.434492857144191,
0.495090074501149,0.558265375769478,0.621440677037807,0.7004435143378),
 .UNSPECIFIED.);
#375=B_SPLINE_CURVE_WITH_KNOTS('',3,(#12923,#12924,#12925,#12926,#12927,
#12928,#12929,#12930,#12931,#12932,#12933,#12934,#12935,#12936,#12937,#12938,
#12939,#12940,#12941,#12942,#12943,#12944),.UNSPECIFIED.,.F.,.F.,(4,2,2,
2,2,2,2,2,2,2,4),(0.0464897534940957,0.0852567806515119,0.170513561303024,
0.246687263103517,0.308657850341199,0.370628437578881,0.432599024816563,
0.494569612054245,0.570743313854739,0.656000094506251,0.694767121663666),
 .UNSPECIFIED.);
#376=B_SPLINE_CURVE_WITH_KNOTS('',3,(#12950,#12951,#12952,#12953,#12954,
#12955,#12956,#12957,#12958,#12959,#12960,#12961,#12962,#12963,#12964,#12965,
#12966,#12967,#12968,#12969,#12970,#12971),.UNSPECIFIED.,.F.,.F.,(4,2,2,
2,2,2,2,2,2,2,4),(0.0464897534940957,0.0852567806515118,0.170513561303024,
0.246687263103517,0.308657850341199,0.370628437578881,0.432599024816563,
0.494569612054245,0.570743313854738,0.65600009450625,0.694767121663666),
 .UNSPECIFIED.);
#377=B_SPLINE_CURVE_WITH_KNOTS('',3,(#12975,#12976,#12977,#12978,#12979,
#12980,#12981,#12982,#12983,#12984,#12985,#12986,#12987,#12988,#12989,#12990,
#12991,#12992,#12993,#12994,#12995,#12996),.UNSPECIFIED.,.F.,.F.,(4,2,2,
2,2,2,2,2,2,2,4),(0.0464897534940957,0.0852567806515119,0.170513561303024,
0.246687263103517,0.308657850341199,0.370628437578881,0.432599024816563,
0.494569612054245,0.570743313854739,0.656000094506251,0.694767121663666),
 .UNSPECIFIED.);
#378=B_SPLINE_CURVE_WITH_KNOTS('',3,(#13000,#13001,#13002,#13003,#13004,
#13005,#13006,#13007,#13008,#13009,#13010,#13011),.UNSPECIFIED.,.F.,.F.,
(4,2,2,2,2,4),(0.0464897534940957,0.0852567806515119,0.170513561303024,
0.246687263103517,0.308657850341199,0.370628437578881),.UNSPECIFIED.);
#379=B_SPLINE_CURVE_WITH_KNOTS('',3,(#13016,#13017,#13018,#13019,#13020,
#13021,#13022,#13023,#13024,#13025,#13026,#13027),.UNSPECIFIED.,.F.,.F.,
(4,2,2,2,2,4),(0.370628437578881,0.432599024816563,0.494569612054245,0.570743313854738,
0.65600009450625,0.694767121663666),.UNSPECIFIED.);
#380=B_SPLINE_CURVE_WITH_KNOTS('',3,(#13031,#13032,#13033,#13034,#13035,
#13036,#13037,#13038,#13039,#13040,#13041,#13042,#13043,#13044,#13045,#13046,
#13047,#13048,#13049,#13050,#13051,#13052),.UNSPECIFIED.,.F.,.F.,(4,2,2,
2,2,2,2,2,2,2,4),(0.0464897534940957,0.0852567806515121,0.170513561303024,
0.246687263103518,0.308657850341199,0.370628437578881,0.432599024816563,
0.494569612054245,0.570743313854738,0.65600009450625,0.694767121663666),
 .UNSPECIFIED.);
#381=B_SPLINE_CURVE_WITH_KNOTS('',3,(#13056,#13057,#13058,#13059,#13060,
#13061,#13062,#13063,#13064,#13065,#13066,#13067,#13068,#13069,#13070,#13071,
#13072,#13073,#13074,#13075,#13076,#13077),.UNSPECIFIED.,.F.,.F.,(4,2,2,
2,2,2,2,2,2,2,4),(0.0464897534940957,0.0852567806515119,0.170513561303024,
0.246687263103517,0.308657850341199,0.370628437578881,0.432599024816563,
0.494569612054245,0.570743313854738,0.65600009450625,0.694767121663667),
 .UNSPECIFIED.);
#382=B_SPLINE_CURVE_WITH_KNOTS('',3,(#13081,#13082,#13083,#13084,#13085,
#13086,#13087,#13088,#13089,#13090,#13091,#13092,#13093,#13094,#13095,#13096,
#13097,#13098,#13099,#13100,#13101,#13102),.UNSPECIFIED.,.F.,.F.,(4,2,2,
2,2,2,2,2,2,2,4),(0.0464897534940957,0.0852567806515119,0.170513561303024,
0.246687263103517,0.308657850341199,0.370628437578881,0.432599024816563,
0.494569612054245,0.570743313854738,0.65600009450625,0.694767121663666),
 .UNSPECIFIED.);
#383=B_SPLINE_CURVE_WITH_KNOTS('',3,(#13106,#13107,#13108,#13109,#13110,
#13111,#13112,#13113,#13114,#13115,#13116,#13117,#13118,#13119,#13120,#13121,
#13122,#13123,#13124,#13125,#13126,#13127),.UNSPECIFIED.,.F.,.F.,(4,2,2,
2,2,2,2,2,2,2,4),(0.0464897534940957,0.0852567806515119,0.170513561303024,
0.246687263103517,0.308657850341199,0.370628437578881,0.432599024816563,
0.494569612054245,0.570743313854739,0.656000094506251,0.694767121663667),
 .UNSPECIFIED.);
#384=B_SPLINE_CURVE_WITH_KNOTS('',3,(#13135,#13136,#13137,#13138,#13139,
#13140,#13141,#13142,#13143,#13144,#13145,#13146,#13147,#13148,#13149,#13150,
#13151,#13152,#13153,#13154,#13155,#13156),.UNSPECIFIED.,.F.,.F.,(4,2,2,
2,2,2,2,2,2,2,4),(0.0473477652366656,0.126350602536658,0.189525903804987,
0.252701205073316,0.313298422430274,0.373895639787232,0.434492857144191,
0.495090074501149,0.558265375769478,0.621440677037807,0.7004435143378),
 .UNSPECIFIED.);
#385=B_SPLINE_CURVE_WITH_KNOTS('',3,(#13164,#13165,#13166,#13167,#13168,
#13169,#13170,#13171,#13172,#13173,#13174,#13175,#13176,#13177,#13178,#13179,
#13180,#13181,#13182,#13183,#13184,#13185),.UNSPECIFIED.,.F.,.F.,(4,2,2,
2,2,2,2,2,2,2,4),(0.0473477652366656,0.126350602536658,0.189525903804987,
0.252701205073317,0.313298422430275,0.373895639787233,0.434492857144191,
0.495090074501149,0.558265375769478,0.621440677037807,0.7004435143378),
 .UNSPECIFIED.);
#386=B_SPLINE_CURVE_WITH_KNOTS('',3,(#13194,#13195,#13196,#13197,#13198,
#13199,#13200,#13201,#13202,#13203,#13204,#13205),.UNSPECIFIED.,.F.,.F.,
(4,2,2,2,2,4),(0.0473477652366656,0.126350602536658,0.189525903804987,0.252701205073316,
0.313298422430275,0.373895639787233),.UNSPECIFIED.);
#387=B_SPLINE_CURVE_WITH_KNOTS('',3,(#13207,#13208,#13209,#13210,#13211,
#13212,#13213,#13214,#13215,#13216,#13217,#13218),.UNSPECIFIED.,.F.,.F.,
(4,2,2,2,2,4),(0.373895639787233,0.434492857144191,0.495090074501149,0.558265375769478,
0.621440677037807,0.7004435143378),.UNSPECIFIED.);
#388=B_SPLINE_CURVE_WITH_KNOTS('',3,(#13225,#13226,#13227,#13228,#13229,
#13230,#13231,#13232,#13233,#13234,#13235,#13236,#13237,#13238,#13239,#13240,
#13241,#13242,#13243,#13244,#13245,#13246),.UNSPECIFIED.,.F.,.F.,(4,2,2,
2,2,2,2,2,2,2,4),(0.0473477652366656,0.126350602536658,0.189525903804987,
0.252701205073316,0.313298422430275,0.373895639787233,0.434492857144191,
0.495090074501149,0.558265375769478,0.621440677037807,0.7004435143378),
 .UNSPECIFIED.);
#389=B_SPLINE_CURVE_WITH_KNOTS('',3,(#13254,#13255,#13256,#13257,#13258,
#13259,#13260,#13261,#13262,#13263,#13264,#13265,#13266,#13267,#13268,#13269,
#13270,#13271,#13272,#13273,#13274,#13275),.UNSPECIFIED.,.F.,.F.,(4,2,2,
2,2,2,2,2,2,2,4),(0.0473477652366656,0.126350602536658,0.189525903804987,
0.252701205073317,0.313298422430275,0.373895639787233,0.434492857144191,
0.495090074501149,0.558265375769478,0.621440677037807,0.7004435143378),
 .UNSPECIFIED.);
#390=B_SPLINE_CURVE_WITH_KNOTS('',3,(#13283,#13284,#13285,#13286,#13287,
#13288,#13289,#13290,#13291,#13292,#13293,#13294,#13295,#13296,#13297,#13298,
#13299,#13300,#13301,#13302,#13303,#13304),.UNSPECIFIED.,.F.,.F.,(4,2,2,
2,2,2,2,2,2,2,4),(0.0473477652366656,0.126350602536658,0.189525903804987,
0.252701205073316,0.313298422430275,0.373895639787233,0.434492857144191,
0.495090074501149,0.558265375769478,0.621440677037807,0.7004435143378),
 .UNSPECIFIED.);
#391=B_SPLINE_CURVE_WITH_KNOTS('',3,(#13313,#13314,#13315,#13316,#13317,
#13318,#13319,#13320,#13321,#13322,#13323,#13324,#13325,#13326,#13327,#13328,
#13329,#13330,#13331,#13332,#13333,#13334),.UNSPECIFIED.,.F.,.F.,(4,2,2,
2,2,2,2,2,2,2,4),(0.0473477652366656,0.126350602536658,0.189525903804987,
0.252701205073317,0.313298422430275,0.373895639787233,0.434492857144191,
0.495090074501149,0.558265375769478,0.621440677037807,0.7004435143378),
 .UNSPECIFIED.);
#392=B_SPLINE_CURVE_WITH_KNOTS('',3,(#13493,#13494,#13495,#13496,#13497,
#13498,#13499,#13500,#13501,#13502,#13503,#13504,#13505,#13506),
 .UNSPECIFIED.,.F.,.F.,(4,2,2,2,2,2,4),(0.618551524396291,0.626563103102765,
0.689203386094988,0.751843669087211,0.814483952079434,0.877124235071657,
0.88513581377813),.UNSPECIFIED.);
#393=B_SPLINE_CURVE_WITH_KNOTS('',3,(#13510,#13511,#13512,#13513,#13514,
#13515,#13516,#13517),.UNSPECIFIED.,.F.,.F.,(4,2,2,4),(0.250614556362404,
0.313254839354627,0.37589512234685,0.383906701053323),.UNSPECIFIED.);
#394=B_SPLINE_CURVE_WITH_KNOTS('',3,(#13521,#13522,#13523,#13524,#13525,
#13526,#13527,#13528,#13529,#13530,#13531,#13532,#13533,#13534,#13535,#13536,
#13537,#13538,#13539,#13540,#13541,#13542,#13543,#13544,#13545,#13546),
 .UNSPECIFIED.,.F.,.F.,(4,2,2,2,2,2,2,2,2,2,2,2,4),(0.,0.0623062782223143,
0.124612556444629,0.186916384615149,0.249220212785669,0.31152404095619,
0.37382786912671,0.436134147349024,0.498440425571339,0.560746703793653,
0.623052982015967,0.685356810186488,0.747660638357008),.UNSPECIFIED.);
#395=B_SPLINE_CURVE_WITH_KNOTS('',3,(#13547,#13548,#13549,#13550,#13551,
#13552,#13553,#13554,#13555,#13556),.UNSPECIFIED.,.F.,.F.,(4,2,2,2,4),(0.747660638357008,
0.809964466527529,0.872268294698049,0.934574572920363,0.996880851142677),
 .UNSPECIFIED.);
#396=B_SPLINE_CURVE_WITH_KNOTS('',3,(#13557,#13558,#13559,#13560,#13561,
#13562,#13563,#13564),.UNSPECIFIED.,.F.,.F.,(4,2,2,4),(0.117322411671485,
0.125333990377958,0.187974273370181,0.250614556362404),.UNSPECIFIED.);
#397=B_SPLINE_CURVE_WITH_KNOTS('',3,(#13821,#13822,#13823,#13824,#13825,
#13826,#13827,#13828,#13829,#13830,#13831,#13832,#13833,#13834),
 .UNSPECIFIED.,.F.,.F.,(4,2,2,2,2,2,4),(0.618551524396293,0.626563103102765,
0.689203386094988,0.751843669087211,0.814483952079434,0.877124235071657,
0.88513581377813),.UNSPECIFIED.);
#398=B_SPLINE_CURVE_WITH_KNOTS('',3,(#13838,#13839,#13840,#13841,#13842,
#13843,#13844,#13845),.UNSPECIFIED.,.F.,.F.,(4,2,2,4),(0.250614556362404,
0.313254839354627,0.37589512234685,0.383906701053323),.UNSPECIFIED.);
#399=B_SPLINE_CURVE_WITH_KNOTS('',3,(#13849,#13850,#13851,#13852,#13853,
#13854,#13855,#13856,#13857,#13858,#13859,#13860,#13861,#13862,#13863,#13864,
#13865,#13866,#13867,#13868,#13869,#13870,#13871,#13872,#13873,#13874),
 .UNSPECIFIED.,.F.,.F.,(4,2,2,2,2,2,2,2,2,2,2,2,4),(0.,0.0623062782223143,
0.124612556444629,0.186916384615149,0.249220212785669,0.31152404095619,
0.37382786912671,0.436134147349024,0.498440425571339,0.560746703793653,
0.623052982015967,0.685356810186488,0.747660638357008),.UNSPECIFIED.);
#400=B_SPLINE_CURVE_WITH_KNOTS('',3,(#13875,#13876,#13877,#13878,#13879,
#13880,#13881,#13882,#13883,#13884),.UNSPECIFIED.,.F.,.F.,(4,2,2,2,4),(0.747660638357008,
0.809964466527528,0.872268294698049,0.934574572920363,0.996880851142677),
 .UNSPECIFIED.);
#401=B_SPLINE_CURVE_WITH_KNOTS('',3,(#13885,#13886,#13887,#13888,#13889,
#13890,#13891,#13892),.UNSPECIFIED.,.F.,.F.,(4,2,2,4),(0.117322411671485,
0.125333990377958,0.187974273370181,0.250614556362404),.UNSPECIFIED.);
#402=SHAPE_REPRESENTATION_RELATIONSHIP('SRR','None',#15070,#446);
#403=SHAPE_REPRESENTATION_RELATIONSHIP('SRR','None',#15071,#447);
#404=SHAPE_REPRESENTATION_RELATIONSHIP('SRR','None',#15072,#448);
#405=SHAPE_REPRESENTATION_RELATIONSHIP('SRR','None',#15073,#449);
#406=SHAPE_REPRESENTATION_RELATIONSHIP('SRR','None',#15074,#450);
#407=SHAPE_REPRESENTATION_RELATIONSHIP('SRR','None',#15075,#451);
#408=SHAPE_REPRESENTATION_RELATIONSHIP('SRR','None',#15076,#452);
#409=SHAPE_REPRESENTATION_RELATIONSHIP('SRR','None',#15077,#453);
#410=SHAPE_REPRESENTATION_RELATIONSHIP('SRR','None',#15079,#454);
#411=SHAPE_REPRESENTATION_RELATIONSHIP('SRR','None',#15080,#455);
#412=SHAPE_REPRESENTATION_RELATIONSHIP('SRR','None',#15081,#456);
#413=SHAPE_REPRESENTATION_RELATIONSHIP('SRR','None',#15082,#457);
#414=SHAPE_REPRESENTATION_RELATIONSHIP('SRR','None',#15083,#458);
#415=SHAPE_REPRESENTATION_RELATIONSHIP('SRR','None',#15085,#459);
#416=SHAPE_REPRESENTATION_RELATIONSHIP('SRR','None',#15086,#460);
#417=SHAPE_REPRESENTATION_RELATIONSHIP('SRR','None',#15087,#461);
#418=SHAPE_REPRESENTATION_RELATIONSHIP('SRR','None',#15088,#462);
#419=SHAPE_REPRESENTATION_RELATIONSHIP('SRR','None',#15089,#463);
#420=SHAPE_REPRESENTATION_RELATIONSHIP('SRR','None',#15090,#464);
#421=SHAPE_REPRESENTATION_RELATIONSHIP('SRR','None',#15091,#465);
#422=SHAPE_REPRESENTATION_RELATIONSHIP('SRR','None',#15092,#466);
#423=SHAPE_REPRESENTATION_RELATIONSHIP('SRR','None',#15093,#467);
#424=SHAPE_REPRESENTATION_RELATIONSHIP('SRR','None',#15095,#468);
#425=SHAPE_REPRESENTATION_RELATIONSHIP('SRR','None',#15096,#469);
#426=SHAPE_REPRESENTATION_RELATIONSHIP('SRR','None',#15097,#470);
#427=SHAPE_REPRESENTATION_RELATIONSHIP('SRR','None',#15098,#471);
#428=SHAPE_REPRESENTATION_RELATIONSHIP('SRR','None',#15099,#472);
#429=SHAPE_REPRESENTATION_RELATIONSHIP('SRR','None',#15100,#473);
#430=SHAPE_REPRESENTATION_RELATIONSHIP('SRR','None',#15101,#474);
#431=SHAPE_REPRESENTATION_RELATIONSHIP('SRR','None',#15102,#475);
#432=SHAPE_REPRESENTATION_RELATIONSHIP('SRR','None',#15104,#476);
#433=SHAPE_REPRESENTATION_RELATIONSHIP('SRR','None',#15106,#477);
#434=SHAPE_REPRESENTATION_RELATIONSHIP('SRR','None',#15107,#478);
#435=SHAPE_REPRESENTATION_RELATIONSHIP('SRR','None',#15108,#479);
#436=SHAPE_REPRESENTATION_RELATIONSHIP('SRR','None',#15110,#480);
#437=SHAPE_REPRESENTATION_RELATIONSHIP('SRR','None',#15111,#481);
#438=SHAPE_REPRESENTATION_RELATIONSHIP('SRR','None',#15112,#482);
#439=SHAPE_REPRESENTATION_RELATIONSHIP('SRR','None',#15113,#483);
#440=SHAPE_REPRESENTATION_RELATIONSHIP('SRR','None',#15114,#484);
#441=SHAPE_REPRESENTATION_RELATIONSHIP('SRR','None',#15116,#485);
#442=SHAPE_REPRESENTATION_RELATIONSHIP('SRR','None',#15117,#486);
#443=SHAPE_REPRESENTATION_RELATIONSHIP('SRR','None',#15118,#487);
#444=SHAPE_REPRESENTATION_RELATIONSHIP('SRR','None',#15119,#488);
#445=SHAPE_REPRESENTATION_RELATIONSHIP('SRR','None',#15120,#489);
#446=ADVANCED_BREP_SHAPE_REPRESENTATION('',(#542),#14827);
#447=ADVANCED_BREP_SHAPE_REPRESENTATION('',(#543),#14828);
#448=ADVANCED_BREP_SHAPE_REPRESENTATION('',(#544),#14829);
#449=ADVANCED_BREP_SHAPE_REPRESENTATION('',(#545),#14830);
#450=ADVANCED_BREP_SHAPE_REPRESENTATION('',(#546),#14831);
#451=ADVANCED_BREP_SHAPE_REPRESENTATION('',(#547),#14832);
#452=ADVANCED_BREP_SHAPE_REPRESENTATION('',(#548),#14833);
#453=ADVANCED_BREP_SHAPE_REPRESENTATION('',(#549),#14834);
#454=ADVANCED_BREP_SHAPE_REPRESENTATION('',(#550),#14836);
#455=ADVANCED_BREP_SHAPE_REPRESENTATION('',(#551),#14837);
#456=ADVANCED_BREP_SHAPE_REPRESENTATION('',(#552,#553,#554,#555,#556,#557,
#558,#559),#14838);
#457=ADVANCED_BREP_SHAPE_REPRESENTATION('',(#560),#14839);
#458=ADVANCED_BREP_SHAPE_REPRESENTATION('',(#561,#562),#14840);
#459=ADVANCED_BREP_SHAPE_REPRESENTATION('',(#563),#14842);
#460=ADVANCED_BREP_SHAPE_REPRESENTATION('',(#564),#14843);
#461=ADVANCED_BREP_SHAPE_REPRESENTATION('',(#565),#14844);
#462=ADVANCED_BREP_SHAPE_REPRESENTATION('',(#566),#14845);
#463=ADVANCED_BREP_SHAPE_REPRESENTATION('',(#567),#14846);
#464=ADVANCED_BREP_SHAPE_REPRESENTATION('',(#568),#14847);
#465=ADVANCED_BREP_SHAPE_REPRESENTATION('',(#569),#14848);
#466=ADVANCED_BREP_SHAPE_REPRESENTATION('',(#570),#14849);
#467=ADVANCED_BREP_SHAPE_REPRESENTATION('',(#14),#14850);
#468=ADVANCED_BREP_SHAPE_REPRESENTATION('',(#571),#14852);
#469=ADVANCED_BREP_SHAPE_REPRESENTATION('',(#572),#14853);
#470=ADVANCED_BREP_SHAPE_REPRESENTATION('',(#573),#14854);
#471=ADVANCED_BREP_SHAPE_REPRESENTATION('',(#574),#14855);
#472=ADVANCED_BREP_SHAPE_REPRESENTATION('',(#575),#14856);
#473=ADVANCED_BREP_SHAPE_REPRESENTATION('',(#576),#14857);
#474=ADVANCED_BREP_SHAPE_REPRESENTATION('',(#577),#14858);
#475=ADVANCED_BREP_SHAPE_REPRESENTATION('',(#578),#14859);
#476=ADVANCED_BREP_SHAPE_REPRESENTATION('',(#579),#14861);
#477=ADVANCED_BREP_SHAPE_REPRESENTATION('',(#580),#14863);
#478=ADVANCED_BREP_SHAPE_REPRESENTATION('',(#581),#14864);
#479=ADVANCED_BREP_SHAPE_REPRESENTATION('',(#582),#14865);
#480=ADVANCED_BREP_SHAPE_REPRESENTATION('',(#583),#14867);
#481=ADVANCED_BREP_SHAPE_REPRESENTATION('',(#584),#14868);
#482=ADVANCED_BREP_SHAPE_REPRESENTATION('',(#585),#14869);
#483=ADVANCED_BREP_SHAPE_REPRESENTATION('',(#586),#14870);
#484=ADVANCED_BREP_SHAPE_REPRESENTATION('',(#587),#14871);
#485=ADVANCED_BREP_SHAPE_REPRESENTATION('',(#588),#14873);
#486=ADVANCED_BREP_SHAPE_REPRESENTATION('',(#589),#14874);
#487=ADVANCED_BREP_SHAPE_REPRESENTATION('',(#590),#14875);
#488=ADVANCED_BREP_SHAPE_REPRESENTATION('',(#15),#14876);
#489=ADVANCED_BREP_SHAPE_REPRESENTATION('',(#16),#14877);
#490=STYLED_ITEM('',(#15385),#542);
#491=STYLED_ITEM('',(#15392),#543);
#492=STYLED_ITEM('',(#15392),#544);
#493=STYLED_ITEM('',(#15406),#545);
#494=STYLED_ITEM('',(#15406),#546);
#495=STYLED_ITEM('',(#15406),#547);
#496=STYLED_ITEM('',(#15406),#548);
#497=STYLED_ITEM('',(#15399),#549);
#498=STYLED_ITEM('',(#15406),#550);
#499=STYLED_ITEM('',(#15406),#551);
#500=STYLED_ITEM('',(#15406),#552);
#501=STYLED_ITEM('',(#15406),#553);
#502=STYLED_ITEM('',(#15406),#554);
#503=STYLED_ITEM('',(#15406),#555);
#504=STYLED_ITEM('',(#15406),#556);
#505=STYLED_ITEM('',(#15406),#557);
#506=STYLED_ITEM('',(#15406),#558);
#507=STYLED_ITEM('',(#15406),#559);
#508=STYLED_ITEM('',(#15406),#560);
#509=STYLED_ITEM('',(#15406),#561);
#510=STYLED_ITEM('',(#15406),#562);
#511=STYLED_ITEM('',(#15399),#563);
#512=STYLED_ITEM('',(#15413),#564);
#513=STYLED_ITEM('',(#15406),#565);
#514=STYLED_ITEM('',(#15406),#566);
#515=STYLED_ITEM('',(#15406),#567);
#516=STYLED_ITEM('',(#15420),#568);
#517=STYLED_ITEM('',(#15406),#569);
#518=STYLED_ITEM('',(#15406),#570);
#519=STYLED_ITEM('',(#15413),#14);
#520=STYLED_ITEM('',(#15399),#571);
#521=STYLED_ITEM('',(#15406),#572);
#522=STYLED_ITEM('',(#15406),#573);
#523=STYLED_ITEM('',(#15406),#574);
#524=STYLED_ITEM('',(#15399),#575);
#525=STYLED_ITEM('',(#15406),#576);
#526=STYLED_ITEM('',(#15406),#577);
#527=STYLED_ITEM('',(#15413),#578);
#528=STYLED_ITEM('',(#15385),#579);
#529=STYLED_ITEM('',(#15399),#580);
#530=STYLED_ITEM('',(#15392),#581);
#531=STYLED_ITEM('',(#15392),#582);
#532=STYLED_ITEM('',(#15420),#583);
#533=STYLED_ITEM('',(#15406),#584);
#534=STYLED_ITEM('',(#15399),#585);
#535=STYLED_ITEM('',(#15406),#586);
#536=STYLED_ITEM('',(#15406),#587);
#537=STYLED_ITEM('',(#15385),#588);
#538=STYLED_ITEM('',(#15399),#589);
#539=STYLED_ITEM('',(#15420),#590);
#540=STYLED_ITEM('',(#15413),#15);
#541=STYLED_ITEM('',(#15413),#16);
#542=MANIFOLD_SOLID_BREP('Body1',#7844);
#543=MANIFOLD_SOLID_BREP('Body1',#7845);
#544=MANIFOLD_SOLID_BREP('Body1',#7846);
#545=MANIFOLD_SOLID_BREP('Body1',#7847);
#546=MANIFOLD_SOLID_BREP('Body1',#7848);
#547=MANIFOLD_SOLID_BREP('Body1',#7849);
#548=MANIFOLD_SOLID_BREP('Body1',#7850);
#549=MANIFOLD_SOLID_BREP('Body1',#7851);
#550=MANIFOLD_SOLID_BREP('Body1',#7852);
#551=MANIFOLD_SOLID_BREP('Body1',#7853);
#552=MANIFOLD_SOLID_BREP('Body1',#7854);
#553=MANIFOLD_SOLID_BREP('Body2',#7855);
#554=MANIFOLD_SOLID_BREP('Body3',#7856);
#555=MANIFOLD_SOLID_BREP('Body4',#7857);
#556=MANIFOLD_SOLID_BREP('Body5',#7858);
#557=MANIFOLD_SOLID_BREP('Body6',#7859);
#558=MANIFOLD_SOLID_BREP('Body7',#7860);
#559=MANIFOLD_SOLID_BREP('Body8',#7861);
#560=MANIFOLD_SOLID_BREP('Continuous crown cage',#7862);
#561=MANIFOLD_SOLID_BREP('Body1',#7863);
#562=MANIFOLD_SOLID_BREP('Body2',#7864);
#563=MANIFOLD_SOLID_BREP('Body1',#7865);
#564=MANIFOLD_SOLID_BREP('Body1',#7866);
#565=MANIFOLD_SOLID_BREP('Body1',#7867);
#566=MANIFOLD_SOLID_BREP('Body1',#7868);
#567=MANIFOLD_SOLID_BREP('Body1',#7869);
#568=MANIFOLD_SOLID_BREP('Body1',#7870);
#569=MANIFOLD_SOLID_BREP('Body1',#7871);
#570=MANIFOLD_SOLID_BREP('Body1',#7872);
#571=MANIFOLD_SOLID_BREP('Body1',#7875);
#572=MANIFOLD_SOLID_BREP('Body1',#7876);
#573=MANIFOLD_SOLID_BREP('Body1',#7877);
#574=MANIFOLD_SOLID_BREP('Body1',#7878);
#575=MANIFOLD_SOLID_BREP('Body1',#7879);
#576=MANIFOLD_SOLID_BREP('Body1',#7880);
#577=MANIFOLD_SOLID_BREP('Body1',#7881);
#578=MANIFOLD_SOLID_BREP('Body1',#7882);
#579=MANIFOLD_SOLID_BREP('Body1',#7883);
#580=MANIFOLD_SOLID_BREP('Body1',#7884);
#581=MANIFOLD_SOLID_BREP('Body1',#7885);
#582=MANIFOLD_SOLID_BREP('Body1',#7886);
#583=MANIFOLD_SOLID_BREP('Body1',#7887);
#584=MANIFOLD_SOLID_BREP('Body1',#7888);
#585=MANIFOLD_SOLID_BREP('Body1',#7889);
#586=MANIFOLD_SOLID_BREP('Body1',#7890);
#587=MANIFOLD_SOLID_BREP('Body1',#7891);
#588=MANIFOLD_SOLID_BREP('Body1',#7892);
#589=MANIFOLD_SOLID_BREP('Body1',#7893);
#590=MANIFOLD_SOLID_BREP('Body1',#7894);
#591=FACE_BOUND('',#1530,.T.);
#592=FACE_BOUND('',#1531,.T.);
#593=FACE_BOUND('',#1532,.T.);
#594=FACE_BOUND('',#1533,.T.);
#595=FACE_BOUND('',#1534,.T.);
#596=FACE_BOUND('',#1535,.T.);
#597=FACE_BOUND('',#1536,.T.);
#598=FACE_BOUND('',#1537,.T.);
#599=FACE_BOUND('',#1538,.T.);
#600=FACE_BOUND('',#1539,.T.);
#601=FACE_BOUND('',#1540,.T.);
#602=FACE_BOUND('',#1541,.T.);
#603=FACE_BOUND('',#1543,.T.);
#604=FACE_BOUND('',#1544,.T.);
#605=FACE_BOUND('',#1545,.T.);
#606=FACE_BOUND('',#1546,.T.);
#607=FACE_BOUND('',#1547,.T.);
#608=FACE_BOUND('',#1548,.T.);
#609=FACE_BOUND('',#1549,.T.);
#610=FACE_BOUND('',#1550,.T.);
#611=FACE_BOUND('',#1551,.T.);
#612=FACE_BOUND('',#1552,.T.);
#613=FACE_BOUND('',#1553,.T.);
#614=FACE_BOUND('',#1554,.T.);
#615=FACE_BOUND('',#1585,.T.);
#616=FACE_BOUND('',#1586,.T.);
#617=FACE_BOUND('',#1587,.T.);
#618=FACE_BOUND('',#1588,.T.);
#619=FACE_BOUND('',#1589,.T.);
#620=FACE_BOUND('',#1597,.T.);
#621=FACE_BOUND('',#1599,.T.);
#622=FACE_BOUND('',#1601,.T.);
#623=FACE_BOUND('',#1603,.T.);
#624=FACE_BOUND('',#1604,.T.);
#625=FACE_BOUND('',#1605,.T.);
#626=FACE_BOUND('',#1606,.T.);
#627=FACE_BOUND('',#1607,.T.);
#628=FACE_BOUND('',#1609,.T.);
#629=FACE_BOUND('',#1610,.T.);
#630=FACE_BOUND('',#1611,.T.);
#631=FACE_BOUND('',#1612,.T.);
#632=FACE_BOUND('',#1613,.T.);
#633=FACE_BOUND('',#1616,.T.);
#634=FACE_BOUND('',#1619,.T.);
#635=FACE_BOUND('',#1622,.T.);
#636=FACE_BOUND('',#1625,.T.);
#637=FACE_BOUND('',#1632,.T.);
#638=FACE_BOUND('',#1636,.T.);
#639=FACE_BOUND('',#1637,.T.);
#640=FACE_BOUND('',#1638,.T.);
#641=FACE_BOUND('',#1639,.T.);
#642=FACE_BOUND('',#1640,.T.);
#643=FACE_BOUND('',#1642,.T.);
#644=FACE_BOUND('',#1643,.T.);
#645=FACE_BOUND('',#1644,.T.);
#646=FACE_BOUND('',#1645,.T.);
#647=FACE_BOUND('',#1646,.T.);
#648=FACE_BOUND('',#1665,.T.);
#649=FACE_BOUND('',#1666,.T.);
#650=FACE_BOUND('',#1667,.T.);
#651=FACE_BOUND('',#1668,.T.);
#652=FACE_BOUND('',#1669,.T.);
#653=FACE_BOUND('',#1677,.T.);
#654=FACE_BOUND('',#1679,.T.);
#655=FACE_BOUND('',#1681,.T.);
#656=FACE_BOUND('',#1683,.T.);
#657=FACE_BOUND('',#1684,.T.);
#658=FACE_BOUND('',#1685,.T.);
#659=FACE_BOUND('',#1686,.T.);
#660=FACE_BOUND('',#1687,.T.);
#661=FACE_BOUND('',#1689,.T.);
#662=FACE_BOUND('',#1690,.T.);
#663=FACE_BOUND('',#1691,.T.);
#664=FACE_BOUND('',#1692,.T.);
#665=FACE_BOUND('',#1693,.T.);
#666=FACE_BOUND('',#1696,.T.);
#667=FACE_BOUND('',#1699,.T.);
#668=FACE_BOUND('',#1702,.T.);
#669=FACE_BOUND('',#1705,.T.);
#670=FACE_BOUND('',#1712,.T.);
#671=FACE_BOUND('',#1716,.T.);
#672=FACE_BOUND('',#1717,.T.);
#673=FACE_BOUND('',#1718,.T.);
#674=FACE_BOUND('',#1719,.T.);
#675=FACE_BOUND('',#1720,.T.);
#676=FACE_BOUND('',#1722,.T.);
#677=FACE_BOUND('',#1723,.T.);
#678=FACE_BOUND('',#1724,.T.);
#679=FACE_BOUND('',#1725,.T.);
#680=FACE_BOUND('',#1726,.T.);
#681=FACE_BOUND('',#1729,.T.);
#682=FACE_BOUND('',#1732,.T.);
#683=FACE_BOUND('',#1735,.T.);
#684=FACE_BOUND('',#1738,.T.);
#685=FACE_BOUND('',#1748,.T.);
#686=FACE_BOUND('',#1749,.T.);
#687=FACE_BOUND('',#1750,.T.);
#688=FACE_BOUND('',#1751,.T.);
#689=FACE_BOUND('',#1758,.T.);
#690=FACE_BOUND('',#1759,.T.);
#691=FACE_BOUND('',#1760,.T.);
#692=FACE_BOUND('',#1761,.T.);
#693=FACE_BOUND('',#1770,.T.);
#694=FACE_BOUND('',#1773,.T.);
#695=FACE_BOUND('',#1778,.T.);
#696=FACE_BOUND('',#1783,.T.);
#697=FACE_BOUND('',#1811,.T.);
#698=FACE_BOUND('',#1814,.T.);
#699=FACE_BOUND('',#1817,.T.);
#700=FACE_BOUND('',#1820,.T.);
#701=FACE_BOUND('',#1823,.T.);
#702=FACE_BOUND('',#1829,.T.);
#703=FACE_BOUND('',#1830,.T.);
#704=FACE_BOUND('',#1831,.T.);
#705=FACE_BOUND('',#1838,.T.);
#706=FACE_BOUND('',#1839,.T.);
#707=FACE_BOUND('',#1843,.T.);
#708=FACE_BOUND('',#1851,.T.);
#709=FACE_BOUND('',#1856,.T.);
#710=FACE_BOUND('',#1858,.T.);
#711=FACE_BOUND('',#1863,.T.);
#712=FACE_BOUND('',#1865,.T.);
#713=FACE_BOUND('',#1867,.T.);
#714=FACE_BOUND('',#1869,.T.);
#715=FACE_BOUND('',#1873,.T.);
#716=FACE_BOUND('',#1875,.T.);
#717=FACE_BOUND('',#1880,.T.);
#718=FACE_BOUND('',#1885,.T.);
#719=FACE_BOUND('',#1887,.T.);
#720=FACE_BOUND('',#1891,.T.);
#721=FACE_BOUND('',#1893,.T.);
#722=FACE_BOUND('',#1897,.T.);
#723=FACE_BOUND('',#1899,.T.);
#724=FACE_BOUND('',#1905,.T.);
#725=FACE_BOUND('',#1925,.T.);
#726=FACE_BOUND('',#1926,.T.);
#727=FACE_BOUND('',#1927,.T.);
#728=FACE_BOUND('',#1932,.T.);
#729=FACE_BOUND('',#1936,.T.);
#730=FACE_BOUND('',#1937,.T.);
#731=FACE_BOUND('',#1942,.T.);
#732=FACE_BOUND('',#1944,.T.);
#733=FACE_BOUND('',#1949,.T.);
#734=FACE_BOUND('',#1951,.T.);
#735=FACE_BOUND('',#1953,.T.);
#736=FACE_BOUND('',#1955,.T.);
#737=FACE_BOUND('',#1959,.T.);
#738=FACE_BOUND('',#1961,.T.);
#739=FACE_BOUND('',#1966,.T.);
#740=FACE_BOUND('',#1971,.T.);
#741=FACE_BOUND('',#1973,.T.);
#742=FACE_BOUND('',#1977,.T.);
#743=FACE_BOUND('',#1979,.T.);
#744=FACE_BOUND('',#1983,.T.);
#745=FACE_BOUND('',#1985,.T.);
#746=FACE_BOUND('',#1995,.T.);
#747=FACE_BOUND('',#2004,.T.);
#748=FACE_BOUND('',#2010,.T.);
#749=FACE_BOUND('',#2020,.T.);
#750=FACE_BOUND('',#2021,.T.);
#751=FACE_BOUND('',#2025,.T.);
#752=FACE_BOUND('',#2026,.T.);
#753=FACE_BOUND('',#2030,.T.);
#754=FACE_BOUND('',#2032,.T.);
#755=FACE_BOUND('',#2036,.T.);
#756=FACE_BOUND('',#2038,.T.);
#757=FACE_BOUND('',#2049,.T.);
#758=FACE_BOUND('',#2050,.T.);
#759=FACE_BOUND('',#2051,.T.);
#760=FACE_BOUND('',#2052,.T.);
#761=FACE_BOUND('',#2053,.T.);
#762=FACE_BOUND('',#2055,.T.);
#763=FACE_BOUND('',#2056,.T.);
#764=FACE_BOUND('',#2057,.T.);
#765=FACE_BOUND('',#2058,.T.);
#766=FACE_BOUND('',#2059,.T.);
#767=FACE_BOUND('',#2063,.T.);
#768=FACE_BOUND('',#2065,.T.);
#769=FACE_BOUND('',#2070,.T.);
#770=FACE_BOUND('',#2075,.T.);
#771=FACE_BOUND('',#2077,.T.);
#772=FACE_BOUND('',#2081,.T.);
#773=FACE_BOUND('',#2083,.T.);
#774=FACE_BOUND('',#2087,.T.);
#775=FACE_BOUND('',#2089,.T.);
#776=FACE_BOUND('',#2104,.T.);
#777=FACE_BOUND('',#2105,.T.);
#778=FACE_BOUND('',#2106,.T.);
#779=FACE_BOUND('',#2107,.T.);
#780=FACE_BOUND('',#2150,.T.);
#781=FACE_BOUND('',#2167,.T.);
#782=PLANE('',#8423);
#783=PLANE('',#8424);
#784=PLANE('',#8425);
#785=PLANE('',#8426);
#786=PLANE('',#8427);
#787=PLANE('',#8428);
#788=PLANE('',#8430);
#789=PLANE('',#8431);
#790=PLANE('',#8432);
#791=PLANE('',#8433);
#792=PLANE('',#8434);
#793=PLANE('',#8435);
#794=PLANE('',#8437);
#795=PLANE('',#8438);
#796=PLANE('',#8439);
#797=PLANE('',#8440);
#798=PLANE('',#8441);
#799=PLANE('',#8442);
#800=PLANE('',#8448);
#801=PLANE('',#8452);
#802=PLANE('',#8456);
#803=PLANE('',#8460);
#804=PLANE('',#8464);
#805=PLANE('',#8469);
#806=PLANE('',#8474);
#807=PLANE('',#8479);
#808=PLANE('',#8481);
#809=PLANE('',#8505);
#810=PLANE('',#8511);
#811=PLANE('',#8512);
#812=PLANE('',#8517);
#813=PLANE('',#8522);
#814=PLANE('',#8527);
#815=PLANE('',#8532);
#816=PLANE('',#8545);
#817=PLANE('',#8552);
#818=PLANE('',#8553);
#819=PLANE('',#8559);
#820=PLANE('',#8563);
#821=PLANE('',#8567);
#822=PLANE('',#8571);
#823=PLANE('',#8575);
#824=PLANE('',#8580);
#825=PLANE('',#8585);
#826=PLANE('',#8590);
#827=PLANE('',#8592);
#828=PLANE('',#8616);
#829=PLANE('',#8622);
#830=PLANE('',#8623);
#831=PLANE('',#8628);
#832=PLANE('',#8633);
#833=PLANE('',#8638);
#834=PLANE('',#8643);
#835=PLANE('',#8656);
#836=PLANE('',#8663);
#837=PLANE('',#8664);
#838=PLANE('',#8669);
#839=PLANE('',#8674);
#840=PLANE('',#8679);
#841=PLANE('',#8684);
#842=PLANE('',#8694);
#843=PLANE('',#8695);
#844=PLANE('',#8696);
#845=PLANE('',#8697);
#846=PLANE('',#8698);
#847=PLANE('',#8699);
#848=PLANE('',#8700);
#849=PLANE('',#8701);
#850=PLANE('',#8702);
#851=PLANE('',#8703);
#852=PLANE('',#8704);
#853=PLANE('',#8705);
#854=PLANE('',#8706);
#855=PLANE('',#8707);
#856=PLANE('',#8723);
#857=PLANE('',#8726);
#858=PLANE('',#8738);
#859=PLANE('',#8747);
#860=PLANE('',#8780);
#861=PLANE('',#8785);
#862=PLANE('',#8790);
#863=PLANE('',#8795);
#864=PLANE('',#8800);
#865=PLANE('',#8805);
#866=PLANE('',#8814);
#867=PLANE('',#8818);
#868=PLANE('',#8819);
#869=PLANE('',#8821);
#870=PLANE('',#8826);
#871=PLANE('',#8829);
#872=PLANE('',#8834);
#873=PLANE('',#8850);
#874=PLANE('',#8851);
#875=PLANE('',#8857);
#876=PLANE('',#8864);
#877=PLANE('',#8865);
#878=PLANE('',#8867);
#879=PLANE('',#8869);
#880=PLANE('',#8875);
#881=PLANE('',#8880);
#882=PLANE('',#8884);
#883=PLANE('',#8885);
#884=PLANE('',#8893);
#885=PLANE('',#8894);
#886=PLANE('',#8896);
#887=PLANE('',#8900);
#888=PLANE('',#8907);
#889=PLANE('',#8908);
#890=PLANE('',#8913);
#891=PLANE('',#8914);
#892=PLANE('',#8917);
#893=PLANE('',#8925);
#894=PLANE('',#8926);
#895=PLANE('',#8934);
#896=PLANE('',#8935);
#897=PLANE('',#8943);
#898=PLANE('',#8944);
#899=PLANE('',#8952);
#900=PLANE('',#8953);
#901=PLANE('',#8955);
#902=PLANE('',#8963);
#903=PLANE('',#8971);
#904=PLANE('',#8972);
#905=PLANE('',#8973);
#906=PLANE('',#8974);
#907=PLANE('',#8975);
#908=PLANE('',#8976);
#909=PLANE('',#8977);
#910=PLANE('',#8978);
#911=PLANE('',#8979);
#912=PLANE('',#8985);
#913=PLANE('',#8986);
#914=PLANE('',#8987);
#915=PLANE('',#8988);
#916=PLANE('',#8992);
#917=PLANE('',#8995);
#918=PLANE('',#8996);
#919=PLANE('',#8999);
#920=PLANE('',#9005);
#921=PLANE('',#9006);
#922=PLANE('',#9014);
#923=PLANE('',#9015);
#924=PLANE('',#9017);
#925=PLANE('',#9021);
#926=PLANE('',#9028);
#927=PLANE('',#9029);
#928=PLANE('',#9034);
#929=PLANE('',#9035);
#930=PLANE('',#9038);
#931=PLANE('',#9046);
#932=PLANE('',#9047);
#933=PLANE('',#9055);
#934=PLANE('',#9056);
#935=PLANE('',#9064);
#936=PLANE('',#9065);
#937=PLANE('',#9073);
#938=PLANE('',#9074);
#939=PLANE('',#9076);
#940=PLANE('',#9078);
#941=PLANE('',#9079);
#942=PLANE('',#9080);
#943=PLANE('',#9081);
#944=PLANE('',#9082);
#945=PLANE('',#9083);
#946=PLANE('',#9084);
#947=PLANE('',#9085);
#948=PLANE('',#9095);
#949=PLANE('',#9096);
#950=PLANE('',#9097);
#951=PLANE('',#9098);
#952=PLANE('',#9099);
#953=PLANE('',#9100);
#954=PLANE('',#9101);
#955=PLANE('',#9102);
#956=PLANE('',#9103);
#957=PLANE('',#9104);
#958=PLANE('',#9105);
#959=PLANE('',#9106);
#960=PLANE('',#9107);
#961=PLANE('',#9108);
#962=PLANE('',#9121);
#963=PLANE('',#9122);
#964=PLANE('',#9124);
#965=PLANE('',#9127);
#966=PLANE('',#9135);
#967=PLANE('',#9136);
#968=PLANE('',#9144);
#969=PLANE('',#9145);
#970=PLANE('',#9166);
#971=PLANE('',#9167);
#972=PLANE('',#9168);
#973=PLANE('',#9169);
#974=PLANE('',#9170);
#975=PLANE('',#9171);
#976=PLANE('',#9176);
#977=PLANE('',#9177);
#978=PLANE('',#9180);
#979=PLANE('',#9188);
#980=PLANE('',#9189);
#981=PLANE('',#9197);
#982=PLANE('',#9198);
#983=PLANE('',#9206);
#984=PLANE('',#9207);
#985=PLANE('',#9215);
#986=PLANE('',#9216);
#987=PLANE('',#9219);
#988=PLANE('',#9225);
#989=PLANE('',#9231);
#990=PLANE('',#9237);
#991=PLANE('',#9243);
#992=PLANE('',#9244);
#993=PLANE('',#9245);
#994=PLANE('',#9246);
#995=PLANE('',#9247);
#996=PLANE('',#9248);
#997=PLANE('',#9249);
#998=PLANE('',#9250);
#999=PLANE('',#9251);
#1000=PLANE('',#9252);
#1001=PLANE('',#9253);
#1002=PLANE('',#9254);
#1003=PLANE('',#9255);
#1004=PLANE('',#9256);
#1005=PLANE('',#9258);
#1006=PLANE('',#9259);
#1007=PLANE('',#9260);
#1008=PLANE('',#9261);
#1009=PLANE('',#9262);
#1010=PLANE('',#9263);
#1011=PLANE('',#9264);
#1012=PLANE('',#9265);
#1013=PLANE('',#9266);
#1014=PLANE('',#9267);
#1015=PLANE('',#9269);
#1016=PLANE('',#9270);
#1017=PLANE('',#9271);
#1018=PLANE('',#9272);
#1019=PLANE('',#9273);
#1020=PLANE('',#9274);
#1021=PLANE('',#9275);
#1022=PLANE('',#9276);
#1023=PLANE('',#9277);
#1024=PLANE('',#9278);
#1025=PLANE('',#9283);
#1026=PLANE('',#9284);
#1027=PLANE('',#9285);
#1028=PLANE('',#9286);
#1029=PLANE('',#9287);
#1030=PLANE('',#9288);
#1031=PLANE('',#9289);
#1032=PLANE('',#9290);
#1033=PLANE('',#9291);
#1034=PLANE('',#9293);
#1035=PLANE('',#9301);
#1036=PLANE('',#9307);
#1037=PLANE('',#9308);
#1038=PLANE('',#9309);
#1039=PLANE('',#9310);
#1040=PLANE('',#9311);
#1041=PLANE('',#9312);
#1042=PLANE('',#9313);
#1043=PLANE('',#9314);
#1044=PLANE('',#9315);
#1045=PLANE('',#9317);
#1046=PLANE('',#9325);
#1047=FACE_OUTER_BOUND('',#1513,.T.);
#1048=FACE_OUTER_BOUND('',#1514,.T.);
#1049=FACE_OUTER_BOUND('',#1515,.T.);
#1050=FACE_OUTER_BOUND('',#1516,.T.);
#1051=FACE_OUTER_BOUND('',#1517,.T.);
#1052=FACE_OUTER_BOUND('',#1518,.T.);
#1053=FACE_OUTER_BOUND('',#1519,.T.);
#1054=FACE_OUTER_BOUND('',#1520,.T.);
#1055=FACE_OUTER_BOUND('',#1521,.T.);
#1056=FACE_OUTER_BOUND('',#1522,.T.);
#1057=FACE_OUTER_BOUND('',#1523,.T.);
#1058=FACE_OUTER_BOUND('',#1524,.T.);
#1059=FACE_OUTER_BOUND('',#1525,.T.);
#1060=FACE_OUTER_BOUND('',#1526,.T.);
#1061=FACE_OUTER_BOUND('',#1527,.T.);
#1062=FACE_OUTER_BOUND('',#1528,.T.);
#1063=FACE_OUTER_BOUND('',#1529,.T.);
#1064=FACE_OUTER_BOUND('',#1542,.T.);
#1065=FACE_OUTER_BOUND('',#1555,.T.);
#1066=FACE_OUTER_BOUND('',#1556,.T.);
#1067=FACE_OUTER_BOUND('',#1557,.T.);
#1068=FACE_OUTER_BOUND('',#1558,.T.);
#1069=FACE_OUTER_BOUND('',#1559,.T.);
#1070=FACE_OUTER_BOUND('',#1560,.T.);
#1071=FACE_OUTER_BOUND('',#1561,.T.);
#1072=FACE_OUTER_BOUND('',#1562,.T.);
#1073=FACE_OUTER_BOUND('',#1563,.T.);
#1074=FACE_OUTER_BOUND('',#1564,.T.);
#1075=FACE_OUTER_BOUND('',#1565,.T.);
#1076=FACE_OUTER_BOUND('',#1566,.T.);
#1077=FACE_OUTER_BOUND('',#1567,.T.);
#1078=FACE_OUTER_BOUND('',#1568,.T.);
#1079=FACE_OUTER_BOUND('',#1569,.T.);
#1080=FACE_OUTER_BOUND('',#1570,.T.);
#1081=FACE_OUTER_BOUND('',#1571,.T.);
#1082=FACE_OUTER_BOUND('',#1572,.T.);
#1083=FACE_OUTER_BOUND('',#1573,.T.);
#1084=FACE_OUTER_BOUND('',#1574,.T.);
#1085=FACE_OUTER_BOUND('',#1575,.T.);
#1086=FACE_OUTER_BOUND('',#1576,.T.);
#1087=FACE_OUTER_BOUND('',#1577,.T.);
#1088=FACE_OUTER_BOUND('',#1578,.T.);
#1089=FACE_OUTER_BOUND('',#1579,.T.);
#1090=FACE_OUTER_BOUND('',#1580,.T.);
#1091=FACE_OUTER_BOUND('',#1581,.T.);
#1092=FACE_OUTER_BOUND('',#1582,.T.);
#1093=FACE_OUTER_BOUND('',#1583,.T.);
#1094=FACE_OUTER_BOUND('',#1584,.T.);
#1095=FACE_OUTER_BOUND('',#1590,.T.);
#1096=FACE_OUTER_BOUND('',#1591,.T.);
#1097=FACE_OUTER_BOUND('',#1592,.T.);
#1098=FACE_OUTER_BOUND('',#1593,.T.);
#1099=FACE_OUTER_BOUND('',#1594,.T.);
#1100=FACE_OUTER_BOUND('',#1595,.T.);
#1101=FACE_OUTER_BOUND('',#1596,.T.);
#1102=FACE_OUTER_BOUND('',#1598,.T.);
#1103=FACE_OUTER_BOUND('',#1600,.T.);
#1104=FACE_OUTER_BOUND('',#1602,.T.);
#1105=FACE_OUTER_BOUND('',#1608,.T.);
#1106=FACE_OUTER_BOUND('',#1614,.T.);
#1107=FACE_OUTER_BOUND('',#1615,.T.);
#1108=FACE_OUTER_BOUND('',#1617,.T.);
#1109=FACE_OUTER_BOUND('',#1618,.T.);
#1110=FACE_OUTER_BOUND('',#1620,.T.);
#1111=FACE_OUTER_BOUND('',#1621,.T.);
#1112=FACE_OUTER_BOUND('',#1623,.T.);
#1113=FACE_OUTER_BOUND('',#1624,.T.);
#1114=FACE_OUTER_BOUND('',#1626,.T.);
#1115=FACE_OUTER_BOUND('',#1627,.T.);
#1116=FACE_OUTER_BOUND('',#1628,.T.);
#1117=FACE_OUTER_BOUND('',#1629,.T.);
#1118=FACE_OUTER_BOUND('',#1630,.T.);
#1119=FACE_OUTER_BOUND('',#1631,.T.);
#1120=FACE_OUTER_BOUND('',#1633,.T.);
#1121=FACE_OUTER_BOUND('',#1634,.T.);
#1122=FACE_OUTER_BOUND('',#1635,.T.);
#1123=FACE_OUTER_BOUND('',#1641,.T.);
#1124=FACE_OUTER_BOUND('',#1647,.T.);
#1125=FACE_OUTER_BOUND('',#1648,.T.);
#1126=FACE_OUTER_BOUND('',#1649,.T.);
#1127=FACE_OUTER_BOUND('',#1650,.T.);
#1128=FACE_OUTER_BOUND('',#1651,.T.);
#1129=FACE_OUTER_BOUND('',#1652,.T.);
#1130=FACE_OUTER_BOUND('',#1653,.T.);
#1131=FACE_OUTER_BOUND('',#1654,.T.);
#1132=FACE_OUTER_BOUND('',#1655,.T.);
#1133=FACE_OUTER_BOUND('',#1656,.T.);
#1134=FACE_OUTER_BOUND('',#1657,.T.);
#1135=FACE_OUTER_BOUND('',#1658,.T.);
#1136=FACE_OUTER_BOUND('',#1659,.T.);
#1137=FACE_OUTER_BOUND('',#1660,.T.);
#1138=FACE_OUTER_BOUND('',#1661,.T.);
#1139=FACE_OUTER_BOUND('',#1662,.T.);
#1140=FACE_OUTER_BOUND('',#1663,.T.);
#1141=FACE_OUTER_BOUND('',#1664,.T.);
#1142=FACE_OUTER_BOUND('',#1670,.T.);
#1143=FACE_OUTER_BOUND('',#1671,.T.);
#1144=FACE_OUTER_BOUND('',#1672,.T.);
#1145=FACE_OUTER_BOUND('',#1673,.T.);
#1146=FACE_OUTER_BOUND('',#1674,.T.);
#1147=FACE_OUTER_BOUND('',#1675,.T.);
#1148=FACE_OUTER_BOUND('',#1676,.T.);
#1149=FACE_OUTER_BOUND('',#1678,.T.);
#1150=FACE_OUTER_BOUND('',#1680,.T.);
#1151=FACE_OUTER_BOUND('',#1682,.T.);
#1152=FACE_OUTER_BOUND('',#1688,.T.);
#1153=FACE_OUTER_BOUND('',#1694,.T.);
#1154=FACE_OUTER_BOUND('',#1695,.T.);
#1155=FACE_OUTER_BOUND('',#1697,.T.);
#1156=FACE_OUTER_BOUND('',#1698,.T.);
#1157=FACE_OUTER_BOUND('',#1700,.T.);
#1158=FACE_OUTER_BOUND('',#1701,.T.);
#1159=FACE_OUTER_BOUND('',#1703,.T.);
#1160=FACE_OUTER_BOUND('',#1704,.T.);
#1161=FACE_OUTER_BOUND('',#1706,.T.);
#1162=FACE_OUTER_BOUND('',#1707,.T.);
#1163=FACE_OUTER_BOUND('',#1708,.T.);
#1164=FACE_OUTER_BOUND('',#1709,.T.);
#1165=FACE_OUTER_BOUND('',#1710,.T.);
#1166=FACE_OUTER_BOUND('',#1711,.T.);
#1167=FACE_OUTER_BOUND('',#1713,.T.);
#1168=FACE_OUTER_BOUND('',#1714,.T.);
#1169=FACE_OUTER_BOUND('',#1715,.T.);
#1170=FACE_OUTER_BOUND('',#1721,.T.);
#1171=FACE_OUTER_BOUND('',#1727,.T.);
#1172=FACE_OUTER_BOUND('',#1728,.T.);
#1173=FACE_OUTER_BOUND('',#1730,.T.);
#1174=FACE_OUTER_BOUND('',#1731,.T.);
#1175=FACE_OUTER_BOUND('',#1733,.T.);
#1176=FACE_OUTER_BOUND('',#1734,.T.);
#1177=FACE_OUTER_BOUND('',#1736,.T.);
#1178=FACE_OUTER_BOUND('',#1737,.T.);
#1179=FACE_OUTER_BOUND('',#1739,.T.);
#1180=FACE_OUTER_BOUND('',#1740,.T.);
#1181=FACE_OUTER_BOUND('',#1741,.T.);
#1182=FACE_OUTER_BOUND('',#1742,.T.);
#1183=FACE_OUTER_BOUND('',#1743,.T.);
#1184=FACE_OUTER_BOUND('',#1744,.T.);
#1185=FACE_OUTER_BOUND('',#1745,.T.);
#1186=FACE_OUTER_BOUND('',#1746,.T.);
#1187=FACE_OUTER_BOUND('',#1747,.T.);
#1188=FACE_OUTER_BOUND('',#1752,.T.);
#1189=FACE_OUTER_BOUND('',#1753,.T.);
#1190=FACE_OUTER_BOUND('',#1754,.T.);
#1191=FACE_OUTER_BOUND('',#1755,.T.);
#1192=FACE_OUTER_BOUND('',#1756,.T.);
#1193=FACE_OUTER_BOUND('',#1757,.T.);
#1194=FACE_OUTER_BOUND('',#1762,.T.);
#1195=FACE_OUTER_BOUND('',#1763,.T.);
#1196=FACE_OUTER_BOUND('',#1764,.T.);
#1197=FACE_OUTER_BOUND('',#1765,.T.);
#1198=FACE_OUTER_BOUND('',#1766,.T.);
#1199=FACE_OUTER_BOUND('',#1767,.T.);
#1200=FACE_OUTER_BOUND('',#1768,.T.);
#1201=FACE_OUTER_BOUND('',#1769,.T.);
#1202=FACE_OUTER_BOUND('',#1771,.T.);
#1203=FACE_OUTER_BOUND('',#1772,.T.);
#1204=FACE_OUTER_BOUND('',#1774,.T.);
#1205=FACE_OUTER_BOUND('',#1775,.T.);
#1206=FACE_OUTER_BOUND('',#1776,.T.);
#1207=FACE_OUTER_BOUND('',#1777,.T.);
#1208=FACE_OUTER_BOUND('',#1779,.T.);
#1209=FACE_OUTER_BOUND('',#1780,.T.);
#1210=FACE_OUTER_BOUND('',#1781,.T.);
#1211=FACE_OUTER_BOUND('',#1782,.T.);
#1212=FACE_OUTER_BOUND('',#1784,.T.);
#1213=FACE_OUTER_BOUND('',#1785,.T.);
#1214=FACE_OUTER_BOUND('',#1786,.T.);
#1215=FACE_OUTER_BOUND('',#1787,.T.);
#1216=FACE_OUTER_BOUND('',#1788,.T.);
#1217=FACE_OUTER_BOUND('',#1789,.T.);
#1218=FACE_OUTER_BOUND('',#1790,.T.);
#1219=FACE_OUTER_BOUND('',#1791,.T.);
#1220=FACE_OUTER_BOUND('',#1792,.T.);
#1221=FACE_OUTER_BOUND('',#1793,.T.);
#1222=FACE_OUTER_BOUND('',#1794,.T.);
#1223=FACE_OUTER_BOUND('',#1795,.T.);
#1224=FACE_OUTER_BOUND('',#1796,.T.);
#1225=FACE_OUTER_BOUND('',#1797,.T.);
#1226=FACE_OUTER_BOUND('',#1798,.T.);
#1227=FACE_OUTER_BOUND('',#1799,.T.);
#1228=FACE_OUTER_BOUND('',#1800,.T.);
#1229=FACE_OUTER_BOUND('',#1801,.T.);
#1230=FACE_OUTER_BOUND('',#1802,.T.);
#1231=FACE_OUTER_BOUND('',#1803,.T.);
#1232=FACE_OUTER_BOUND('',#1804,.T.);
#1233=FACE_OUTER_BOUND('',#1805,.T.);
#1234=FACE_OUTER_BOUND('',#1806,.T.);
#1235=FACE_OUTER_BOUND('',#1807,.T.);
#1236=FACE_OUTER_BOUND('',#1808,.T.);
#1237=FACE_OUTER_BOUND('',#1809,.T.);
#1238=FACE_OUTER_BOUND('',#1810,.T.);
#1239=FACE_OUTER_BOUND('',#1812,.T.);
#1240=FACE_OUTER_BOUND('',#1813,.T.);
#1241=FACE_OUTER_BOUND('',#1815,.T.);
#1242=FACE_OUTER_BOUND('',#1816,.T.);
#1243=FACE_OUTER_BOUND('',#1818,.T.);
#1244=FACE_OUTER_BOUND('',#1819,.T.);
#1245=FACE_OUTER_BOUND('',#1821,.T.);
#1246=FACE_OUTER_BOUND('',#1822,.T.);
#1247=FACE_OUTER_BOUND('',#1824,.T.);
#1248=FACE_OUTER_BOUND('',#1825,.T.);
#1249=FACE_OUTER_BOUND('',#1826,.T.);
#1250=FACE_OUTER_BOUND('',#1827,.T.);
#1251=FACE_OUTER_BOUND('',#1828,.T.);
#1252=FACE_OUTER_BOUND('',#1832,.T.);
#1253=FACE_OUTER_BOUND('',#1833,.T.);
#1254=FACE_OUTER_BOUND('',#1834,.T.);
#1255=FACE_OUTER_BOUND('',#1835,.T.);
#1256=FACE_OUTER_BOUND('',#1836,.T.);
#1257=FACE_OUTER_BOUND('',#1837,.T.);
#1258=FACE_OUTER_BOUND('',#1840,.T.);
#1259=FACE_OUTER_BOUND('',#1841,.T.);
#1260=FACE_OUTER_BOUND('',#1842,.T.);
#1261=FACE_OUTER_BOUND('',#1844,.T.);
#1262=FACE_OUTER_BOUND('',#1845,.T.);
#1263=FACE_OUTER_BOUND('',#1846,.T.);
#1264=FACE_OUTER_BOUND('',#1847,.T.);
#1265=FACE_OUTER_BOUND('',#1848,.T.);
#1266=FACE_OUTER_BOUND('',#1849,.T.);
#1267=FACE_OUTER_BOUND('',#1850,.T.);
#1268=FACE_OUTER_BOUND('',#1852,.T.);
#1269=FACE_OUTER_BOUND('',#1853,.T.);
#1270=FACE_OUTER_BOUND('',#1854,.T.);
#1271=FACE_OUTER_BOUND('',#1855,.T.);
#1272=FACE_OUTER_BOUND('',#1857,.T.);
#1273=FACE_OUTER_BOUND('',#1859,.T.);
#1274=FACE_OUTER_BOUND('',#1860,.T.);
#1275=FACE_OUTER_BOUND('',#1861,.T.);
#1276=FACE_OUTER_BOUND('',#1862,.T.);
#1277=FACE_OUTER_BOUND('',#1864,.T.);
#1278=FACE_OUTER_BOUND('',#1866,.T.);
#1279=FACE_OUTER_BOUND('',#1868,.T.);
#1280=FACE_OUTER_BOUND('',#1870,.T.);
#1281=FACE_OUTER_BOUND('',#1871,.T.);
#1282=FACE_OUTER_BOUND('',#1872,.T.);
#1283=FACE_OUTER_BOUND('',#1874,.T.);
#1284=FACE_OUTER_BOUND('',#1876,.T.);
#1285=FACE_OUTER_BOUND('',#1877,.T.);
#1286=FACE_OUTER_BOUND('',#1878,.T.);
#1287=FACE_OUTER_BOUND('',#1879,.T.);
#1288=FACE_OUTER_BOUND('',#1881,.T.);
#1289=FACE_OUTER_BOUND('',#1882,.T.);
#1290=FACE_OUTER_BOUND('',#1883,.T.);
#1291=FACE_OUTER_BOUND('',#1884,.T.);
#1292=FACE_OUTER_BOUND('',#1886,.T.);
#1293=FACE_OUTER_BOUND('',#1888,.T.);
#1294=FACE_OUTER_BOUND('',#1889,.T.);
#1295=FACE_OUTER_BOUND('',#1890,.T.);
#1296=FACE_OUTER_BOUND('',#1892,.T.);
#1297=FACE_OUTER_BOUND('',#1894,.T.);
#1298=FACE_OUTER_BOUND('',#1895,.T.);
#1299=FACE_OUTER_BOUND('',#1896,.T.);
#1300=FACE_OUTER_BOUND('',#1898,.T.);
#1301=FACE_OUTER_BOUND('',#1900,.T.);
#1302=FACE_OUTER_BOUND('',#1901,.T.);
#1303=FACE_OUTER_BOUND('',#1902,.T.);
#1304=FACE_OUTER_BOUND('',#1903,.T.);
#1305=FACE_OUTER_BOUND('',#1904,.T.);
#1306=FACE_OUTER_BOUND('',#1906,.T.);
#1307=FACE_OUTER_BOUND('',#1907,.T.);
#1308=FACE_OUTER_BOUND('',#1908,.T.);
#1309=FACE_OUTER_BOUND('',#1909,.T.);
#1310=FACE_OUTER_BOUND('',#1910,.T.);
#1311=FACE_OUTER_BOUND('',#1911,.T.);
#1312=FACE_OUTER_BOUND('',#1912,.T.);
#1313=FACE_OUTER_BOUND('',#1913,.T.);
#1314=FACE_OUTER_BOUND('',#1914,.T.);
#1315=FACE_OUTER_BOUND('',#1915,.T.);
#1316=FACE_OUTER_BOUND('',#1916,.T.);
#1317=FACE_OUTER_BOUND('',#1917,.T.);
#1318=FACE_OUTER_BOUND('',#1918,.T.);
#1319=FACE_OUTER_BOUND('',#1919,.T.);
#1320=FACE_OUTER_BOUND('',#1920,.T.);
#1321=FACE_OUTER_BOUND('',#1921,.T.);
#1322=FACE_OUTER_BOUND('',#1922,.T.);
#1323=FACE_OUTER_BOUND('',#1923,.T.);
#1324=FACE_OUTER_BOUND('',#1924,.T.);
#1325=FACE_OUTER_BOUND('',#1928,.T.);
#1326=FACE_OUTER_BOUND('',#1929,.T.);
#1327=FACE_OUTER_BOUND('',#1930,.T.);
#1328=FACE_OUTER_BOUND('',#1931,.T.);
#1329=FACE_OUTER_BOUND('',#1933,.T.);
#1330=FACE_OUTER_BOUND('',#1934,.T.);
#1331=FACE_OUTER_BOUND('',#1935,.T.);
#1332=FACE_OUTER_BOUND('',#1938,.T.);
#1333=FACE_OUTER_BOUND('',#1939,.T.);
#1334=FACE_OUTER_BOUND('',#1940,.T.);
#1335=FACE_OUTER_BOUND('',#1941,.T.);
#1336=FACE_OUTER_BOUND('',#1943,.T.);
#1337=FACE_OUTER_BOUND('',#1945,.T.);
#1338=FACE_OUTER_BOUND('',#1946,.T.);
#1339=FACE_OUTER_BOUND('',#1947,.T.);
#1340=FACE_OUTER_BOUND('',#1948,.T.);
#1341=FACE_OUTER_BOUND('',#1950,.T.);
#1342=FACE_OUTER_BOUND('',#1952,.T.);
#1343=FACE_OUTER_BOUND('',#1954,.T.);
#1344=FACE_OUTER_BOUND('',#1956,.T.);
#1345=FACE_OUTER_BOUND('',#1957,.T.);
#1346=FACE_OUTER_BOUND('',#1958,.T.);
#1347=FACE_OUTER_BOUND('',#1960,.T.);
#1348=FACE_OUTER_BOUND('',#1962,.T.);
#1349=FACE_OUTER_BOUND('',#1963,.T.);
#1350=FACE_OUTER_BOUND('',#1964,.T.);
#1351=FACE_OUTER_BOUND('',#1965,.T.);
#1352=FACE_OUTER_BOUND('',#1967,.T.);
#1353=FACE_OUTER_BOUND('',#1968,.T.);
#1354=FACE_OUTER_BOUND('',#1969,.T.);
#1355=FACE_OUTER_BOUND('',#1970,.T.);
#1356=FACE_OUTER_BOUND('',#1972,.T.);
#1357=FACE_OUTER_BOUND('',#1974,.T.);
#1358=FACE_OUTER_BOUND('',#1975,.T.);
#1359=FACE_OUTER_BOUND('',#1976,.T.);
#1360=FACE_OUTER_BOUND('',#1978,.T.);
#1361=FACE_OUTER_BOUND('',#1980,.T.);
#1362=FACE_OUTER_BOUND('',#1981,.T.);
#1363=FACE_OUTER_BOUND('',#1982,.T.);
#1364=FACE_OUTER_BOUND('',#1984,.T.);
#1365=FACE_OUTER_BOUND('',#1986,.T.);
#1366=FACE_OUTER_BOUND('',#1987,.T.);
#1367=FACE_OUTER_BOUND('',#1988,.T.);
#1368=FACE_OUTER_BOUND('',#1989,.T.);
#1369=FACE_OUTER_BOUND('',#1990,.T.);
#1370=FACE_OUTER_BOUND('',#1991,.T.);
#1371=FACE_OUTER_BOUND('',#1992,.T.);
#1372=FACE_OUTER_BOUND('',#1993,.T.);
#1373=FACE_OUTER_BOUND('',#1994,.T.);
#1374=FACE_OUTER_BOUND('',#1996,.T.);
#1375=FACE_OUTER_BOUND('',#1997,.T.);
#1376=FACE_OUTER_BOUND('',#1998,.T.);
#1377=FACE_OUTER_BOUND('',#1999,.T.);
#1378=FACE_OUTER_BOUND('',#2000,.T.);
#1379=FACE_OUTER_BOUND('',#2001,.T.);
#1380=FACE_OUTER_BOUND('',#2002,.T.);
#1381=FACE_OUTER_BOUND('',#2003,.T.);
#1382=FACE_OUTER_BOUND('',#2005,.T.);
#1383=FACE_OUTER_BOUND('',#2006,.T.);
#1384=FACE_OUTER_BOUND('',#2007,.T.);
#1385=FACE_OUTER_BOUND('',#2008,.T.);
#1386=FACE_OUTER_BOUND('',#2009,.T.);
#1387=FACE_OUTER_BOUND('',#2011,.T.);
#1388=FACE_OUTER_BOUND('',#2012,.T.);
#1389=FACE_OUTER_BOUND('',#2013,.T.);
#1390=FACE_OUTER_BOUND('',#2014,.T.);
#1391=FACE_OUTER_BOUND('',#2015,.T.);
#1392=FACE_OUTER_BOUND('',#2016,.T.);
#1393=FACE_OUTER_BOUND('',#2017,.T.);
#1394=FACE_OUTER_BOUND('',#2018,.T.);
#1395=FACE_OUTER_BOUND('',#2019,.T.);
#1396=FACE_OUTER_BOUND('',#2022,.T.);
#1397=FACE_OUTER_BOUND('',#2023,.T.);
#1398=FACE_OUTER_BOUND('',#2024,.T.);
#1399=FACE_OUTER_BOUND('',#2027,.T.);
#1400=FACE_OUTER_BOUND('',#2028,.T.);
#1401=FACE_OUTER_BOUND('',#2029,.T.);
#1402=FACE_OUTER_BOUND('',#2031,.T.);
#1403=FACE_OUTER_BOUND('',#2033,.T.);
#1404=FACE_OUTER_BOUND('',#2034,.T.);
#1405=FACE_OUTER_BOUND('',#2035,.T.);
#1406=FACE_OUTER_BOUND('',#2037,.T.);
#1407=FACE_OUTER_BOUND('',#2039,.T.);
#1408=FACE_OUTER_BOUND('',#2040,.T.);
#1409=FACE_OUTER_BOUND('',#2041,.T.);
#1410=FACE_OUTER_BOUND('',#2042,.T.);
#1411=FACE_OUTER_BOUND('',#2043,.T.);
#1412=FACE_OUTER_BOUND('',#2044,.T.);
#1413=FACE_OUTER_BOUND('',#2045,.T.);
#1414=FACE_OUTER_BOUND('',#2046,.T.);
#1415=FACE_OUTER_BOUND('',#2047,.T.);
#1416=FACE_OUTER_BOUND('',#2048,.T.);
#1417=FACE_OUTER_BOUND('',#2054,.T.);
#1418=FACE_OUTER_BOUND('',#2060,.T.);
#1419=FACE_OUTER_BOUND('',#2061,.T.);
#1420=FACE_OUTER_BOUND('',#2062,.T.);
#1421=FACE_OUTER_BOUND('',#2064,.T.);
#1422=FACE_OUTER_BOUND('',#2066,.T.);
#1423=FACE_OUTER_BOUND('',#2067,.T.);
#1424=FACE_OUTER_BOUND('',#2068,.T.);
#1425=FACE_OUTER_BOUND('',#2069,.T.);
#1426=FACE_OUTER_BOUND('',#2071,.T.);
#1427=FACE_OUTER_BOUND('',#2072,.T.);
#1428=FACE_OUTER_BOUND('',#2073,.T.);
#1429=FACE_OUTER_BOUND('',#2074,.T.);
#1430=FACE_OUTER_BOUND('',#2076,.T.);
#1431=FACE_OUTER_BOUND('',#2078,.T.);
#1432=FACE_OUTER_BOUND('',#2079,.T.);
#1433=FACE_OUTER_BOUND('',#2080,.T.);
#1434=FACE_OUTER_BOUND('',#2082,.T.);
#1435=FACE_OUTER_BOUND('',#2084,.T.);
#1436=FACE_OUTER_BOUND('',#2085,.T.);
#1437=FACE_OUTER_BOUND('',#2086,.T.);
#1438=FACE_OUTER_BOUND('',#2088,.T.);
#1439=FACE_OUTER_BOUND('',#2090,.T.);
#1440=FACE_OUTER_BOUND('',#2091,.T.);
#1441=FACE_OUTER_BOUND('',#2092,.T.);
#1442=FACE_OUTER_BOUND('',#2093,.T.);
#1443=FACE_OUTER_BOUND('',#2094,.T.);
#1444=FACE_OUTER_BOUND('',#2095,.T.);
#1445=FACE_OUTER_BOUND('',#2096,.T.);
#1446=FACE_OUTER_BOUND('',#2097,.T.);
#1447=FACE_OUTER_BOUND('',#2098,.T.);
#1448=FACE_OUTER_BOUND('',#2099,.T.);
#1449=FACE_OUTER_BOUND('',#2100,.T.);
#1450=FACE_OUTER_BOUND('',#2101,.T.);
#1451=FACE_OUTER_BOUND('',#2102,.T.);
#1452=FACE_OUTER_BOUND('',#2103,.T.);
#1453=FACE_OUTER_BOUND('',#2108,.T.);
#1454=FACE_OUTER_BOUND('',#2109,.T.);
#1455=FACE_OUTER_BOUND('',#2110,.T.);
#1456=FACE_OUTER_BOUND('',#2111,.T.);
#1457=FACE_OUTER_BOUND('',#2112,.T.);
#1458=FACE_OUTER_BOUND('',#2113,.T.);
#1459=FACE_OUTER_BOUND('',#2114,.T.);
#1460=FACE_OUTER_BOUND('',#2115,.T.);
#1461=FACE_OUTER_BOUND('',#2116,.T.);
#1462=FACE_OUTER_BOUND('',#2117,.T.);
#1463=FACE_OUTER_BOUND('',#2118,.T.);
#1464=FACE_OUTER_BOUND('',#2119,.T.);
#1465=FACE_OUTER_BOUND('',#2120,.T.);
#1466=FACE_OUTER_BOUND('',#2121,.T.);
#1467=FACE_OUTER_BOUND('',#2122,.T.);
#1468=FACE_OUTER_BOUND('',#2123,.T.);
#1469=FACE_OUTER_BOUND('',#2124,.T.);
#1470=FACE_OUTER_BOUND('',#2125,.T.);
#1471=FACE_OUTER_BOUND('',#2126,.T.);
#1472=FACE_OUTER_BOUND('',#2127,.T.);
#1473=FACE_OUTER_BOUND('',#2128,.T.);
#1474=FACE_OUTER_BOUND('',#2129,.T.);
#1475=FACE_OUTER_BOUND('',#2130,.T.);
#1476=FACE_OUTER_BOUND('',#2131,.T.);
#1477=FACE_OUTER_BOUND('',#2132,.T.);
#1478=FACE_OUTER_BOUND('',#2133,.T.);
#1479=FACE_OUTER_BOUND('',#2134,.T.);
#1480=FACE_OUTER_BOUND('',#2135,.T.);
#1481=FACE_OUTER_BOUND('',#2136,.T.);
#1482=FACE_OUTER_BOUND('',#2137,.T.);
#1483=FACE_OUTER_BOUND('',#2138,.T.);
#1484=FACE_OUTER_BOUND('',#2139,.T.);
#1485=FACE_OUTER_BOUND('',#2140,.T.);
#1486=FACE_OUTER_BOUND('',#2141,.T.);
#1487=FACE_OUTER_BOUND('',#2142,.T.);
#1488=FACE_OUTER_BOUND('',#2143,.T.);
#1489=FACE_OUTER_BOUND('',#2144,.T.);
#1490=FACE_OUTER_BOUND('',#2145,.T.);
#1491=FACE_OUTER_BOUND('',#2146,.T.);
#1492=FACE_OUTER_BOUND('',#2147,.T.);
#1493=FACE_OUTER_BOUND('',#2148,.T.);
#1494=FACE_OUTER_BOUND('',#2149,.T.);
#1495=FACE_OUTER_BOUND('',#2151,.T.);
#1496=FACE_OUTER_BOUND('',#2152,.T.);
#1497=FACE_OUTER_BOUND('',#2153,.T.);
#1498=FACE_OUTER_BOUND('',#2154,.T.);
#1499=FACE_OUTER_BOUND('',#2155,.T.);
#1500=FACE_OUTER_BOUND('',#2156,.T.);
#1501=FACE_OUTER_BOUND('',#2157,.T.);
#1502=FACE_OUTER_BOUND('',#2158,.T.);
#1503=FACE_OUTER_BOUND('',#2159,.T.);
#1504=FACE_OUTER_BOUND('',#2160,.T.);
#1505=FACE_OUTER_BOUND('',#2161,.T.);
#1506=FACE_OUTER_BOUND('',#2162,.T.);
#1507=FACE_OUTER_BOUND('',#2163,.T.);
#1508=FACE_OUTER_BOUND('',#2164,.T.);
#1509=FACE_OUTER_BOUND('',#2165,.T.);
#1510=FACE_OUTER_BOUND('',#2166,.T.);
#1511=FACE_OUTER_BOUND('',#2168,.T.);
#1512=FACE_OUTER_BOUND('',#2169,.T.);
#1513=EDGE_LOOP('',(#5262,#5263,#5264,#5265));
#1514=EDGE_LOOP('',(#5266,#5267,#5268,#5269));
#1515=EDGE_LOOP('',(#5270,#5271,#5272,#5273));
#1516=EDGE_LOOP('',(#5274,#5275,#5276,#5277));
#1517=EDGE_LOOP('',(#5278,#5279,#5280,#5281));
#1518=EDGE_LOOP('',(#5282,#5283,#5284,#5285));
#1519=EDGE_LOOP('',(#5286,#5287,#5288,#5289));
#1520=EDGE_LOOP('',(#5290,#5291,#5292,#5293));
#1521=EDGE_LOOP('',(#5294,#5295,#5296,#5297));
#1522=EDGE_LOOP('',(#5298,#5299,#5300,#5301));
#1523=EDGE_LOOP('',(#5302,#5303,#5304,#5305));
#1524=EDGE_LOOP('',(#5306,#5307,#5308,#5309));
#1525=EDGE_LOOP('',(#5310,#5311,#5312,#5313));
#1526=EDGE_LOOP('',(#5314,#5315,#5316,#5317));
#1527=EDGE_LOOP('',(#5318,#5319,#5320,#5321));
#1528=EDGE_LOOP('',(#5322,#5323,#5324,#5325));
#1529=EDGE_LOOP('',(#5326,#5327,#5328,#5329));
#1530=EDGE_LOOP('',(#5330));
#1531=EDGE_LOOP('',(#5331));
#1532=EDGE_LOOP('',(#5332));
#1533=EDGE_LOOP('',(#5333));
#1534=EDGE_LOOP('',(#5334));
#1535=EDGE_LOOP('',(#5335));
#1536=EDGE_LOOP('',(#5336));
#1537=EDGE_LOOP('',(#5337));
#1538=EDGE_LOOP('',(#5338));
#1539=EDGE_LOOP('',(#5339));
#1540=EDGE_LOOP('',(#5340));
#1541=EDGE_LOOP('',(#5341));
#1542=EDGE_LOOP('',(#5342,#5343,#5344,#5345));
#1543=EDGE_LOOP('',(#5346));
#1544=EDGE_LOOP('',(#5347));
#1545=EDGE_LOOP('',(#5348));
#1546=EDGE_LOOP('',(#5349));
#1547=EDGE_LOOP('',(#5350));
#1548=EDGE_LOOP('',(#5351));
#1549=EDGE_LOOP('',(#5352));
#1550=EDGE_LOOP('',(#5353));
#1551=EDGE_LOOP('',(#5354));
#1552=EDGE_LOOP('',(#5355));
#1553=EDGE_LOOP('',(#5356));
#1554=EDGE_LOOP('',(#5357));
#1555=EDGE_LOOP('',(#5358,#5359,#5360,#5361));
#1556=EDGE_LOOP('',(#5362,#5363,#5364,#5365));
#1557=EDGE_LOOP('',(#5366,#5367,#5368,#5369));
#1558=EDGE_LOOP('',(#5370,#5371,#5372,#5373));
#1559=EDGE_LOOP('',(#5374,#5375,#5376,#5377));
#1560=EDGE_LOOP('',(#5378,#5379,#5380,#5381));
#1561=EDGE_LOOP('',(#5382,#5383,#5384,#5385));
#1562=EDGE_LOOP('',(#5386,#5387,#5388,#5389));
#1563=EDGE_LOOP('',(#5390,#5391,#5392,#5393));
#1564=EDGE_LOOP('',(#5394,#5395,#5396,#5397));
#1565=EDGE_LOOP('',(#5398,#5399,#5400,#5401));
#1566=EDGE_LOOP('',(#5402,#5403,#5404,#5405));
#1567=EDGE_LOOP('',(#5406,#5407,#5408,#5409,#5410,#5411));
#1568=EDGE_LOOP('',(#5412,#5413,#5414,#5415));
#1569=EDGE_LOOP('',(#5416));
#1570=EDGE_LOOP('',(#5417,#5418,#5419,#5420));
#1571=EDGE_LOOP('',(#5421));
#1572=EDGE_LOOP('',(#5422,#5423,#5424,#5425));
#1573=EDGE_LOOP('',(#5426));
#1574=EDGE_LOOP('',(#5427,#5428,#5429,#5430));
#1575=EDGE_LOOP('',(#5431));
#1576=EDGE_LOOP('',(#5432,#5433,#5434,#5435));
#1577=EDGE_LOOP('',(#5436,#5437));
#1578=EDGE_LOOP('',(#5438,#5439,#5440,#5441));
#1579=EDGE_LOOP('',(#5442,#5443));
#1580=EDGE_LOOP('',(#5444,#5445,#5446,#5447));
#1581=EDGE_LOOP('',(#5448,#5449));
#1582=EDGE_LOOP('',(#5450,#5451,#5452,#5453));
#1583=EDGE_LOOP('',(#5454,#5455));
#1584=EDGE_LOOP('',(#5456));
#1585=EDGE_LOOP('',(#5457,#5458,#5459,#5460,#5461,#5462,#5463,#5464,#5465));
#1586=EDGE_LOOP('',(#5466));
#1587=EDGE_LOOP('',(#5467));
#1588=EDGE_LOOP('',(#5468));
#1589=EDGE_LOOP('',(#5469));
#1590=EDGE_LOOP('',(#5470,#5471,#5472,#5473));
#1591=EDGE_LOOP('',(#5474,#5475,#5476,#5477));
#1592=EDGE_LOOP('',(#5478,#5479,#5480,#5481));
#1593=EDGE_LOOP('',(#5482,#5483,#5484,#5485));
#1594=EDGE_LOOP('',(#5486,#5487,#5488,#5489,#5490,#5491,#5492,#5493,#5494,
#5495,#5496,#5497,#5498,#5499,#5500,#5501,#5502,#5503,#5504,#5505));
#1595=EDGE_LOOP('',(#5506,#5507,#5508,#5509));
#1596=EDGE_LOOP('',(#5510));
#1597=EDGE_LOOP('',(#5511));
#1598=EDGE_LOOP('',(#5512,#5513,#5514,#5515));
#1599=EDGE_LOOP('',(#5516,#5517));
#1600=EDGE_LOOP('',(#5518,#5519,#5520,#5521));
#1601=EDGE_LOOP('',(#5522,#5523));
#1602=EDGE_LOOP('',(#5524));
#1603=EDGE_LOOP('',(#5525));
#1604=EDGE_LOOP('',(#5526));
#1605=EDGE_LOOP('',(#5527));
#1606=EDGE_LOOP('',(#5528));
#1607=EDGE_LOOP('',(#5529));
#1608=EDGE_LOOP('',(#5530));
#1609=EDGE_LOOP('',(#5531));
#1610=EDGE_LOOP('',(#5532));
#1611=EDGE_LOOP('',(#5533));
#1612=EDGE_LOOP('',(#5534));
#1613=EDGE_LOOP('',(#5535));
#1614=EDGE_LOOP('',(#5536,#5537,#5538,#5539));
#1615=EDGE_LOOP('',(#5540));
#1616=EDGE_LOOP('',(#5541));
#1617=EDGE_LOOP('',(#5542,#5543,#5544,#5545));
#1618=EDGE_LOOP('',(#5546));
#1619=EDGE_LOOP('',(#5547));
#1620=EDGE_LOOP('',(#5548,#5549,#5550,#5551));
#1621=EDGE_LOOP('',(#5552));
#1622=EDGE_LOOP('',(#5553));
#1623=EDGE_LOOP('',(#5554,#5555,#5556,#5557));
#1624=EDGE_LOOP('',(#5558));
#1625=EDGE_LOOP('',(#5559));
#1626=EDGE_LOOP('',(#5560,#5561,#5562,#5563));
#1627=EDGE_LOOP('',(#5564,#5565,#5566,#5567));
#1628=EDGE_LOOP('',(#5568,#5569,#5570,#5571));
#1629=EDGE_LOOP('',(#5572,#5573,#5574,#5575));
#1630=EDGE_LOOP('',(#5576,#5577,#5578,#5579));
#1631=EDGE_LOOP('',(#5580));
#1632=EDGE_LOOP('',(#5581));
#1633=EDGE_LOOP('',(#5582,#5583,#5584,#5585));
#1634=EDGE_LOOP('',(#5586,#5587,#5588,#5589));
#1635=EDGE_LOOP('',(#5590));
#1636=EDGE_LOOP('',(#5591));
#1637=EDGE_LOOP('',(#5592));
#1638=EDGE_LOOP('',(#5593));
#1639=EDGE_LOOP('',(#5594));
#1640=EDGE_LOOP('',(#5595));
#1641=EDGE_LOOP('',(#5596));
#1642=EDGE_LOOP('',(#5597));
#1643=EDGE_LOOP('',(#5598));
#1644=EDGE_LOOP('',(#5599));
#1645=EDGE_LOOP('',(#5600));
#1646=EDGE_LOOP('',(#5601));
#1647=EDGE_LOOP('',(#5602,#5603,#5604,#5605,#5606,#5607));
#1648=EDGE_LOOP('',(#5608,#5609,#5610,#5611));
#1649=EDGE_LOOP('',(#5612));
#1650=EDGE_LOOP('',(#5613,#5614,#5615,#5616));
#1651=EDGE_LOOP('',(#5617));
#1652=EDGE_LOOP('',(#5618,#5619,#5620,#5621));
#1653=EDGE_LOOP('',(#5622));
#1654=EDGE_LOOP('',(#5623,#5624,#5625,#5626));
#1655=EDGE_LOOP('',(#5627));
#1656=EDGE_LOOP('',(#5628,#5629,#5630,#5631));
#1657=EDGE_LOOP('',(#5632,#5633));
#1658=EDGE_LOOP('',(#5634,#5635,#5636,#5637));
#1659=EDGE_LOOP('',(#5638,#5639));
#1660=EDGE_LOOP('',(#5640,#5641,#5642,#5643));
#1661=EDGE_LOOP('',(#5644,#5645));
#1662=EDGE_LOOP('',(#5646,#5647,#5648,#5649));
#1663=EDGE_LOOP('',(#5650,#5651));
#1664=EDGE_LOOP('',(#5652));
#1665=EDGE_LOOP('',(#5653,#5654,#5655,#5656,#5657,#5658,#5659,#5660,#5661));
#1666=EDGE_LOOP('',(#5662));
#1667=EDGE_LOOP('',(#5663));
#1668=EDGE_LOOP('',(#5664));
#1669=EDGE_LOOP('',(#5665));
#1670=EDGE_LOOP('',(#5666,#5667,#5668,#5669));
#1671=EDGE_LOOP('',(#5670,#5671,#5672,#5673));
#1672=EDGE_LOOP('',(#5674,#5675,#5676,#5677));
#1673=EDGE_LOOP('',(#5678,#5679,#5680,#5681));
#1674=EDGE_LOOP('',(#5682,#5683,#5684,#5685,#5686,#5687,#5688,#5689,#5690,
#5691,#5692,#5693,#5694,#5695,#5696,#5697,#5698,#5699,#5700,#5701));
#1675=EDGE_LOOP('',(#5702,#5703,#5704,#5705));
#1676=EDGE_LOOP('',(#5706));
#1677=EDGE_LOOP('',(#5707));
#1678=EDGE_LOOP('',(#5708,#5709,#5710,#5711));
#1679=EDGE_LOOP('',(#5712,#5713));
#1680=EDGE_LOOP('',(#5714,#5715,#5716,#5717));
#1681=EDGE_LOOP('',(#5718,#5719));
#1682=EDGE_LOOP('',(#5720));
#1683=EDGE_LOOP('',(#5721));
#1684=EDGE_LOOP('',(#5722));
#1685=EDGE_LOOP('',(#5723));
#1686=EDGE_LOOP('',(#5724));
#1687=EDGE_LOOP('',(#5725));
#1688=EDGE_LOOP('',(#5726));
#1689=EDGE_LOOP('',(#5727));
#1690=EDGE_LOOP('',(#5728));
#1691=EDGE_LOOP('',(#5729));
#1692=EDGE_LOOP('',(#5730));
#1693=EDGE_LOOP('',(#5731));
#1694=EDGE_LOOP('',(#5732,#5733,#5734,#5735));
#1695=EDGE_LOOP('',(#5736));
#1696=EDGE_LOOP('',(#5737));
#1697=EDGE_LOOP('',(#5738,#5739,#5740,#5741));
#1698=EDGE_LOOP('',(#5742));
#1699=EDGE_LOOP('',(#5743));
#1700=EDGE_LOOP('',(#5744,#5745,#5746,#5747));
#1701=EDGE_LOOP('',(#5748));
#1702=EDGE_LOOP('',(#5749));
#1703=EDGE_LOOP('',(#5750,#5751,#5752,#5753));
#1704=EDGE_LOOP('',(#5754));
#1705=EDGE_LOOP('',(#5755));
#1706=EDGE_LOOP('',(#5756,#5757,#5758,#5759));
#1707=EDGE_LOOP('',(#5760,#5761,#5762,#5763));
#1708=EDGE_LOOP('',(#5764,#5765,#5766,#5767));
#1709=EDGE_LOOP('',(#5768,#5769,#5770,#5771));
#1710=EDGE_LOOP('',(#5772,#5773,#5774,#5775));
#1711=EDGE_LOOP('',(#5776));
#1712=EDGE_LOOP('',(#5777));
#1713=EDGE_LOOP('',(#5778,#5779,#5780,#5781));
#1714=EDGE_LOOP('',(#5782,#5783,#5784,#5785));
#1715=EDGE_LOOP('',(#5786));
#1716=EDGE_LOOP('',(#5787));
#1717=EDGE_LOOP('',(#5788));
#1718=EDGE_LOOP('',(#5789));
#1719=EDGE_LOOP('',(#5790));
#1720=EDGE_LOOP('',(#5791));
#1721=EDGE_LOOP('',(#5792));
#1722=EDGE_LOOP('',(#5793));
#1723=EDGE_LOOP('',(#5794));
#1724=EDGE_LOOP('',(#5795));
#1725=EDGE_LOOP('',(#5796));
#1726=EDGE_LOOP('',(#5797));
#1727=EDGE_LOOP('',(#5798,#5799,#5800,#5801));
#1728=EDGE_LOOP('',(#5802));
#1729=EDGE_LOOP('',(#5803));
#1730=EDGE_LOOP('',(#5804,#5805,#5806,#5807));
#1731=EDGE_LOOP('',(#5808));
#1732=EDGE_LOOP('',(#5809));
#1733=EDGE_LOOP('',(#5810,#5811,#5812,#5813));
#1734=EDGE_LOOP('',(#5814));
#1735=EDGE_LOOP('',(#5815));
#1736=EDGE_LOOP('',(#5816,#5817,#5818,#5819));
#1737=EDGE_LOOP('',(#5820));
#1738=EDGE_LOOP('',(#5821));
#1739=EDGE_LOOP('',(#5822,#5823,#5824,#5825));
#1740=EDGE_LOOP('',(#5826,#5827,#5828,#5829));
#1741=EDGE_LOOP('',(#5830,#5831,#5832,#5833));
#1742=EDGE_LOOP('',(#5834,#5835,#5836,#5837));
#1743=EDGE_LOOP('',(#5838,#5839,#5840,#5841));
#1744=EDGE_LOOP('',(#5842,#5843,#5844,#5845));
#1745=EDGE_LOOP('',(#5846,#5847,#5848,#5849));
#1746=EDGE_LOOP('',(#5850,#5851,#5852,#5853));
#1747=EDGE_LOOP('',(#5854,#5855,#5856,#5857));
#1748=EDGE_LOOP('',(#5858));
#1749=EDGE_LOOP('',(#5859));
#1750=EDGE_LOOP('',(#5860));
#1751=EDGE_LOOP('',(#5861));
#1752=EDGE_LOOP('',(#5862,#5863,#5864,#5865));
#1753=EDGE_LOOP('',(#5866,#5867,#5868,#5869));
#1754=EDGE_LOOP('',(#5870,#5871,#5872,#5873));
#1755=EDGE_LOOP('',(#5874,#5875,#5876,#5877));
#1756=EDGE_LOOP('',(#5878,#5879,#5880,#5881));
#1757=EDGE_LOOP('',(#5882,#5883,#5884,#5885));
#1758=EDGE_LOOP('',(#5886));
#1759=EDGE_LOOP('',(#5887));
#1760=EDGE_LOOP('',(#5888));
#1761=EDGE_LOOP('',(#5889));
#1762=EDGE_LOOP('',(#5890,#5891,#5892,#5893));
#1763=EDGE_LOOP('',(#5894,#5895,#5896,#5897,#5898,#5899,#5900,#5901,#5902,
#5903,#5904,#5905));
#1764=EDGE_LOOP('',(#5906,#5907,#5908,#5909,#5910,#5911,#5912,#5913,#5914,
#5915,#5916,#5917));
#1765=EDGE_LOOP('',(#5918,#5919,#5920,#5921,#5922,#5923));
#1766=EDGE_LOOP('',(#5924,#5925,#5926,#5927,#5928));
#1767=EDGE_LOOP('',(#5929,#5930,#5931,#5932));
#1768=EDGE_LOOP('',(#5933,#5934,#5935,#5936));
#1769=EDGE_LOOP('',(#5937));
#1770=EDGE_LOOP('',(#5938));
#1771=EDGE_LOOP('',(#5939,#5940,#5941,#5942,#5943));
#1772=EDGE_LOOP('',(#5944));
#1773=EDGE_LOOP('',(#5945));
#1774=EDGE_LOOP('',(#5946,#5947,#5948,#5949));
#1775=EDGE_LOOP('',(#5950,#5951,#5952,#5953,#5954,#5955));
#1776=EDGE_LOOP('',(#5956,#5957,#5958,#5959,#5960));
#1777=EDGE_LOOP('',(#5961));
#1778=EDGE_LOOP('',(#5962));
#1779=EDGE_LOOP('',(#5963,#5964,#5965,#5966));
#1780=EDGE_LOOP('',(#5967,#5968,#5969,#5970));
#1781=EDGE_LOOP('',(#5971,#5972,#5973,#5974));
#1782=EDGE_LOOP('',(#5975));
#1783=EDGE_LOOP('',(#5976));
#1784=EDGE_LOOP('',(#5977,#5978,#5979,#5980,#5981));
#1785=EDGE_LOOP('',(#5982,#5983));
#1786=EDGE_LOOP('',(#5984,#5985));
#1787=EDGE_LOOP('',(#5986,#5987));
#1788=EDGE_LOOP('',(#5988,#5989));
#1789=EDGE_LOOP('',(#5990,#5991));
#1790=EDGE_LOOP('',(#5992,#5993));
#1791=EDGE_LOOP('',(#5994,#5995));
#1792=EDGE_LOOP('',(#5996,#5997));
#1793=EDGE_LOOP('',(#5998,#5999,#6000,#6001));
#1794=EDGE_LOOP('',(#6002,#6003,#6004,#6005,#6006,#6007,#6008,#6009,#6010,
#6011,#6012,#6013,#6014,#6015,#6016,#6017,#6018,#6019,#6020,#6021));
#1795=EDGE_LOOP('',(#6022,#6023,#6024,#6025));
#1796=EDGE_LOOP('',(#6026,#6027,#6028,#6029));
#1797=EDGE_LOOP('',(#6030,#6031,#6032,#6033));
#1798=EDGE_LOOP('',(#6034,#6035,#6036,#6037));
#1799=EDGE_LOOP('',(#6038,#6039,#6040,#6041));
#1800=EDGE_LOOP('',(#6042,#6043,#6044,#6045,#6046,#6047));
#1801=EDGE_LOOP('',(#6048,#6049,#6050,#6051));
#1802=EDGE_LOOP('',(#6052,#6053,#6054,#6055));
#1803=EDGE_LOOP('',(#6056,#6057,#6058,#6059));
#1804=EDGE_LOOP('',(#6060,#6061,#6062,#6063));
#1805=EDGE_LOOP('',(#6064,#6065,#6066,#6067));
#1806=EDGE_LOOP('',(#6068,#6069,#6070,#6071));
#1807=EDGE_LOOP('',(#6072,#6073,#6074,#6075,#6076,#6077,#6078,#6079,#6080,
#6081,#6082,#6083,#6084,#6085,#6086,#6087,#6088,#6089,#6090,#6091));
#1808=EDGE_LOOP('',(#6092,#6093,#6094,#6095));
#1809=EDGE_LOOP('',(#6096,#6097,#6098,#6099));
#1810=EDGE_LOOP('',(#6100));
#1811=EDGE_LOOP('',(#6101));
#1812=EDGE_LOOP('',(#6102,#6103,#6104,#6105));
#1813=EDGE_LOOP('',(#6106));
#1814=EDGE_LOOP('',(#6107));
#1815=EDGE_LOOP('',(#6108,#6109,#6110,#6111));
#1816=EDGE_LOOP('',(#6112));
#1817=EDGE_LOOP('',(#6113));
#1818=EDGE_LOOP('',(#6114,#6115,#6116,#6117));
#1819=EDGE_LOOP('',(#6118));
#1820=EDGE_LOOP('',(#6119));
#1821=EDGE_LOOP('',(#6120,#6121,#6122,#6123));
#1822=EDGE_LOOP('',(#6124));
#1823=EDGE_LOOP('',(#6125));
#1824=EDGE_LOOP('',(#6126,#6127,#6128,#6129));
#1825=EDGE_LOOP('',(#6130,#6131,#6132,#6133));
#1826=EDGE_LOOP('',(#6134,#6135,#6136,#6137));
#1827=EDGE_LOOP('',(#6138,#6139,#6140,#6141));
#1828=EDGE_LOOP('',(#6142,#6143,#6144,#6145,#6146,#6147,#6148,#6149));
#1829=EDGE_LOOP('',(#6150));
#1830=EDGE_LOOP('',(#6151));
#1831=EDGE_LOOP('',(#6152));
#1832=EDGE_LOOP('',(#6153,#6154,#6155,#6156));
#1833=EDGE_LOOP('',(#6157,#6158,#6159,#6160));
#1834=EDGE_LOOP('',(#6161,#6162,#6163,#6164));
#1835=EDGE_LOOP('',(#6165,#6166,#6167,#6168));
#1836=EDGE_LOOP('',(#6169,#6170,#6171,#6172));
#1837=EDGE_LOOP('',(#6173,#6174,#6175,#6176,#6177,#6178,#6179,#6180));
#1838=EDGE_LOOP('',(#6181));
#1839=EDGE_LOOP('',(#6182));
#1840=EDGE_LOOP('',(#6183,#6184,#6185,#6186));
#1841=EDGE_LOOP('',(#6187,#6188,#6189,#6190));
#1842=EDGE_LOOP('',(#6191));
#1843=EDGE_LOOP('',(#6192));
#1844=EDGE_LOOP('',(#6193,#6194,#6195,#6196));
#1845=EDGE_LOOP('',(#6197,#6198,#6199,#6200));
#1846=EDGE_LOOP('',(#6201));
#1847=EDGE_LOOP('',(#6202,#6203,#6204,#6205));
#1848=EDGE_LOOP('',(#6206));
#1849=EDGE_LOOP('',(#6207,#6208,#6209,#6210));
#1850=EDGE_LOOP('',(#6211));
#1851=EDGE_LOOP('',(#6212));
#1852=EDGE_LOOP('',(#6213));
#1853=EDGE_LOOP('',(#6214,#6215,#6216,#6217));
#1854=EDGE_LOOP('',(#6218,#6219,#6220,#6221));
#1855=EDGE_LOOP('',(#6222));
#1856=EDGE_LOOP('',(#6223));
#1857=EDGE_LOOP('',(#6224));
#1858=EDGE_LOOP('',(#6225));
#1859=EDGE_LOOP('',(#6226,#6227));
#1860=EDGE_LOOP('',(#6228,#6229,#6230,#6231,#6232,#6233,#6234,#6235,#6236));
#1861=EDGE_LOOP('',(#6237,#6238));
#1862=EDGE_LOOP('',(#6239,#6240,#6241,#6242));
#1863=EDGE_LOOP('',(#6243,#6244,#6245,#6246,#6247));
#1864=EDGE_LOOP('',(#6248,#6249,#6250,#6251));
#1865=EDGE_LOOP('',(#6252,#6253));
#1866=EDGE_LOOP('',(#6254));
#1867=EDGE_LOOP('',(#6255));
#1868=EDGE_LOOP('',(#6256));
#1869=EDGE_LOOP('',(#6257));
#1870=EDGE_LOOP('',(#6258,#6259,#6260,#6261));
#1871=EDGE_LOOP('',(#6262));
#1872=EDGE_LOOP('',(#6263));
#1873=EDGE_LOOP('',(#6264));
#1874=EDGE_LOOP('',(#6265));
#1875=EDGE_LOOP('',(#6266));
#1876=EDGE_LOOP('',(#6267,#6268,#6269,#6270));
#1877=EDGE_LOOP('',(#6271,#6272,#6273,#6274));
#1878=EDGE_LOOP('',(#6275,#6276,#6277,#6278));
#1879=EDGE_LOOP('',(#6279));
#1880=EDGE_LOOP('',(#6280));
#1881=EDGE_LOOP('',(#6281));
#1882=EDGE_LOOP('',(#6282,#6283,#6284,#6285));
#1883=EDGE_LOOP('',(#6286,#6287,#6288,#6289));
#1884=EDGE_LOOP('',(#6290));
#1885=EDGE_LOOP('',(#6291));
#1886=EDGE_LOOP('',(#6292));
#1887=EDGE_LOOP('',(#6293));
#1888=EDGE_LOOP('',(#6294,#6295,#6296,#6297));
#1889=EDGE_LOOP('',(#6298,#6299,#6300,#6301));
#1890=EDGE_LOOP('',(#6302));
#1891=EDGE_LOOP('',(#6303));
#1892=EDGE_LOOP('',(#6304));
#1893=EDGE_LOOP('',(#6305));
#1894=EDGE_LOOP('',(#6306,#6307,#6308,#6309));
#1895=EDGE_LOOP('',(#6310,#6311,#6312,#6313));
#1896=EDGE_LOOP('',(#6314));
#1897=EDGE_LOOP('',(#6315));
#1898=EDGE_LOOP('',(#6316));
#1899=EDGE_LOOP('',(#6317));
#1900=EDGE_LOOP('',(#6318));
#1901=EDGE_LOOP('',(#6319,#6320,#6321,#6322));
#1902=EDGE_LOOP('',(#6323,#6324,#6325,#6326));
#1903=EDGE_LOOP('',(#6327,#6328,#6329,#6330));
#1904=EDGE_LOOP('',(#6331));
#1905=EDGE_LOOP('',(#6332));
#1906=EDGE_LOOP('',(#6333,#6334,#6335,#6336));
#1907=EDGE_LOOP('',(#6337,#6338,#6339,#6340));
#1908=EDGE_LOOP('',(#6341,#6342,#6343,#6344));
#1909=EDGE_LOOP('',(#6345));
#1910=EDGE_LOOP('',(#6346,#6347,#6348,#6349));
#1911=EDGE_LOOP('',(#6350,#6351,#6352,#6353));
#1912=EDGE_LOOP('',(#6354,#6355,#6356,#6357));
#1913=EDGE_LOOP('',(#6358,#6359,#6360,#6361));
#1914=EDGE_LOOP('',(#6362,#6363,#6364,#6365));
#1915=EDGE_LOOP('',(#6366,#6367,#6368,#6369));
#1916=EDGE_LOOP('',(#6370,#6371,#6372,#6373,#6374,#6375));
#1917=EDGE_LOOP('',(#6376,#6377,#6378,#6379,#6380,#6381));
#1918=EDGE_LOOP('',(#6382,#6383,#6384,#6385));
#1919=EDGE_LOOP('',(#6386,#6387,#6388,#6389));
#1920=EDGE_LOOP('',(#6390,#6391,#6392,#6393));
#1921=EDGE_LOOP('',(#6394,#6395,#6396,#6397));
#1922=EDGE_LOOP('',(#6398,#6399,#6400,#6401));
#1923=EDGE_LOOP('',(#6402,#6403,#6404,#6405));
#1924=EDGE_LOOP('',(#6406,#6407,#6408,#6409));
#1925=EDGE_LOOP('',(#6410));
#1926=EDGE_LOOP('',(#6411,#6412,#6413,#6414));
#1927=EDGE_LOOP('',(#6415));
#1928=EDGE_LOOP('',(#6416,#6417,#6418,#6419));
#1929=EDGE_LOOP('',(#6420,#6421,#6422,#6423));
#1930=EDGE_LOOP('',(#6424,#6425,#6426,#6427));
#1931=EDGE_LOOP('',(#6428));
#1932=EDGE_LOOP('',(#6429));
#1933=EDGE_LOOP('',(#6430,#6431,#6432,#6433));
#1934=EDGE_LOOP('',(#6434,#6435,#6436,#6437));
#1935=EDGE_LOOP('',(#6438,#6439,#6440,#6441));
#1936=EDGE_LOOP('',(#6442));
#1937=EDGE_LOOP('',(#6443,#6444,#6445,#6446));
#1938=EDGE_LOOP('',(#6447));
#1939=EDGE_LOOP('',(#6448,#6449,#6450,#6451));
#1940=EDGE_LOOP('',(#6452,#6453,#6454,#6455));
#1941=EDGE_LOOP('',(#6456));
#1942=EDGE_LOOP('',(#6457));
#1943=EDGE_LOOP('',(#6458));
#1944=EDGE_LOOP('',(#6459));
#1945=EDGE_LOOP('',(#6460,#6461));
#1946=EDGE_LOOP('',(#6462,#6463,#6464,#6465,#6466,#6467,#6468,#6469,#6470));
#1947=EDGE_LOOP('',(#6471,#6472));
#1948=EDGE_LOOP('',(#6473,#6474,#6475,#6476));
#1949=EDGE_LOOP('',(#6477,#6478,#6479,#6480,#6481));
#1950=EDGE_LOOP('',(#6482,#6483,#6484,#6485));
#1951=EDGE_LOOP('',(#6486,#6487));
#1952=EDGE_LOOP('',(#6488));
#1953=EDGE_LOOP('',(#6489));
#1954=EDGE_LOOP('',(#6490));
#1955=EDGE_LOOP('',(#6491));
#1956=EDGE_LOOP('',(#6492,#6493,#6494,#6495));
#1957=EDGE_LOOP('',(#6496));
#1958=EDGE_LOOP('',(#6497));
#1959=EDGE_LOOP('',(#6498));
#1960=EDGE_LOOP('',(#6499));
#1961=EDGE_LOOP('',(#6500));
#1962=EDGE_LOOP('',(#6501,#6502,#6503,#6504));
#1963=EDGE_LOOP('',(#6505,#6506,#6507,#6508));
#1964=EDGE_LOOP('',(#6509,#6510,#6511,#6512));
#1965=EDGE_LOOP('',(#6513));
#1966=EDGE_LOOP('',(#6514));
#1967=EDGE_LOOP('',(#6515));
#1968=EDGE_LOOP('',(#6516,#6517,#6518,#6519));
#1969=EDGE_LOOP('',(#6520,#6521,#6522,#6523));
#1970=EDGE_LOOP('',(#6524));
#1971=EDGE_LOOP('',(#6525));
#1972=EDGE_LOOP('',(#6526));
#1973=EDGE_LOOP('',(#6527));
#1974=EDGE_LOOP('',(#6528,#6529,#6530,#6531));
#1975=EDGE_LOOP('',(#6532,#6533,#6534,#6535));
#1976=EDGE_LOOP('',(#6536));
#1977=EDGE_LOOP('',(#6537));
#1978=EDGE_LOOP('',(#6538));
#1979=EDGE_LOOP('',(#6539));
#1980=EDGE_LOOP('',(#6540,#6541,#6542,#6543));
#1981=EDGE_LOOP('',(#6544,#6545,#6546,#6547));
#1982=EDGE_LOOP('',(#6548));
#1983=EDGE_LOOP('',(#6549));
#1984=EDGE_LOOP('',(#6550));
#1985=EDGE_LOOP('',(#6551));
#1986=EDGE_LOOP('',(#6552));
#1987=EDGE_LOOP('',(#6553,#6554,#6555,#6556));
#1988=EDGE_LOOP('',(#6557,#6558,#6559,#6560));
#1989=EDGE_LOOP('',(#6561,#6562,#6563,#6564));
#1990=EDGE_LOOP('',(#6565,#6566,#6567,#6568));
#1991=EDGE_LOOP('',(#6569,#6570,#6571,#6572));
#1992=EDGE_LOOP('',(#6573,#6574,#6575,#6576));
#1993=EDGE_LOOP('',(#6577,#6578,#6579,#6580,#6581,#6582));
#1994=EDGE_LOOP('',(#6583));
#1995=EDGE_LOOP('',(#6584,#6585,#6586,#6587,#6588,#6589));
#1996=EDGE_LOOP('',(#6590,#6591,#6592,#6593));
#1997=EDGE_LOOP('',(#6594,#6595,#6596,#6597));
#1998=EDGE_LOOP('',(#6598,#6599,#6600,#6601));
#1999=EDGE_LOOP('',(#6602,#6603,#6604,#6605));
#2000=EDGE_LOOP('',(#6606,#6607,#6608,#6609));
#2001=EDGE_LOOP('',(#6610,#6611,#6612,#6613));
#2002=EDGE_LOOP('',(#6614,#6615,#6616,#6617));
#2003=EDGE_LOOP('',(#6618,#6619,#6620,#6621));
#2004=EDGE_LOOP('',(#6622));
#2005=EDGE_LOOP('',(#6623,#6624,#6625,#6626));
#2006=EDGE_LOOP('',(#6627,#6628,#6629,#6630));
#2007=EDGE_LOOP('',(#6631,#6632,#6633,#6634));
#2008=EDGE_LOOP('',(#6635,#6636,#6637,#6638));
#2009=EDGE_LOOP('',(#6639,#6640,#6641,#6642));
#2010=EDGE_LOOP('',(#6643));
#2011=EDGE_LOOP('',(#6644,#6645,#6646,#6647,#6648,#6649,#6650,#6651,#6652,
#6653,#6654,#6655));
#2012=EDGE_LOOP('',(#6656,#6657,#6658,#6659));
#2013=EDGE_LOOP('',(#6660,#6661,#6662,#6663,#6664,#6665,#6666,#6667,#6668,
#6669,#6670,#6671));
#2014=EDGE_LOOP('',(#6672,#6673,#6674,#6675));
#2015=EDGE_LOOP('',(#6676,#6677,#6678,#6679));
#2016=EDGE_LOOP('',(#6680,#6681,#6682,#6683));
#2017=EDGE_LOOP('',(#6684,#6685,#6686,#6687));
#2018=EDGE_LOOP('',(#6688,#6689,#6690,#6691));
#2019=EDGE_LOOP('',(#6692,#6693,#6694,#6695));
#2020=EDGE_LOOP('',(#6696));
#2021=EDGE_LOOP('',(#6697));
#2022=EDGE_LOOP('',(#6698,#6699,#6700,#6701));
#2023=EDGE_LOOP('',(#6702,#6703,#6704,#6705));
#2024=EDGE_LOOP('',(#6706,#6707,#6708,#6709));
#2025=EDGE_LOOP('',(#6710));
#2026=EDGE_LOOP('',(#6711));
#2027=EDGE_LOOP('',(#6712,#6713,#6714,#6715));
#2028=EDGE_LOOP('',(#6716,#6717,#6718,#6719));
#2029=EDGE_LOOP('',(#6720));
#2030=EDGE_LOOP('',(#6721));
#2031=EDGE_LOOP('',(#6722));
#2032=EDGE_LOOP('',(#6723));
#2033=EDGE_LOOP('',(#6724,#6725,#6726,#6727));
#2034=EDGE_LOOP('',(#6728,#6729,#6730,#6731));
#2035=EDGE_LOOP('',(#6732));
#2036=EDGE_LOOP('',(#6733));
#2037=EDGE_LOOP('',(#6734));
#2038=EDGE_LOOP('',(#6735));
#2039=EDGE_LOOP('',(#6736,#6737,#6738,#6739));
#2040=EDGE_LOOP('',(#6740,#6741,#6742,#6743));
#2041=EDGE_LOOP('',(#6744,#6745,#6746,#6747));
#2042=EDGE_LOOP('',(#6748,#6749,#6750,#6751));
#2043=EDGE_LOOP('',(#6752,#6753,#6754,#6755));
#2044=EDGE_LOOP('',(#6756,#6757,#6758,#6759));
#2045=EDGE_LOOP('',(#6760,#6761,#6762,#6763));
#2046=EDGE_LOOP('',(#6764,#6765,#6766,#6767));
#2047=EDGE_LOOP('',(#6768,#6769,#6770,#6771));
#2048=EDGE_LOOP('',(#6772,#6773,#6774,#6775));
#2049=EDGE_LOOP('',(#6776));
#2050=EDGE_LOOP('',(#6777));
#2051=EDGE_LOOP('',(#6778));
#2052=EDGE_LOOP('',(#6779));
#2053=EDGE_LOOP('',(#6780));
#2054=EDGE_LOOP('',(#6781,#6782,#6783,#6784));
#2055=EDGE_LOOP('',(#6785));
#2056=EDGE_LOOP('',(#6786));
#2057=EDGE_LOOP('',(#6787));
#2058=EDGE_LOOP('',(#6788));
#2059=EDGE_LOOP('',(#6789));
#2060=EDGE_LOOP('',(#6790,#6791,#6792,#6793));
#2061=EDGE_LOOP('',(#6794));
#2062=EDGE_LOOP('',(#6795));
#2063=EDGE_LOOP('',(#6796));
#2064=EDGE_LOOP('',(#6797));
#2065=EDGE_LOOP('',(#6798));
#2066=EDGE_LOOP('',(#6799,#6800,#6801,#6802));
#2067=EDGE_LOOP('',(#6803,#6804,#6805,#6806));
#2068=EDGE_LOOP('',(#6807,#6808,#6809,#6810));
#2069=EDGE_LOOP('',(#6811));
#2070=EDGE_LOOP('',(#6812));
#2071=EDGE_LOOP('',(#6813));
#2072=EDGE_LOOP('',(#6814,#6815,#6816,#6817));
#2073=EDGE_LOOP('',(#6818,#6819,#6820,#6821));
#2074=EDGE_LOOP('',(#6822));
#2075=EDGE_LOOP('',(#6823));
#2076=EDGE_LOOP('',(#6824));
#2077=EDGE_LOOP('',(#6825));
#2078=EDGE_LOOP('',(#6826,#6827,#6828,#6829));
#2079=EDGE_LOOP('',(#6830,#6831,#6832,#6833));
#2080=EDGE_LOOP('',(#6834));
#2081=EDGE_LOOP('',(#6835));
#2082=EDGE_LOOP('',(#6836));
#2083=EDGE_LOOP('',(#6837));
#2084=EDGE_LOOP('',(#6838,#6839,#6840,#6841));
#2085=EDGE_LOOP('',(#6842,#6843,#6844,#6845));
#2086=EDGE_LOOP('',(#6846));
#2087=EDGE_LOOP('',(#6847));
#2088=EDGE_LOOP('',(#6848));
#2089=EDGE_LOOP('',(#6849));
#2090=EDGE_LOOP('',(#6850,#6851));
#2091=EDGE_LOOP('',(#6852,#6853,#6854,#6855,#6856,#6857,#6858,#6859));
#2092=EDGE_LOOP('',(#6860,#6861));
#2093=EDGE_LOOP('',(#6862,#6863,#6864,#6865,#6866,#6867,#6868,#6869));
#2094=EDGE_LOOP('',(#6870,#6871));
#2095=EDGE_LOOP('',(#6872,#6873,#6874,#6875,#6876,#6877,#6878,#6879));
#2096=EDGE_LOOP('',(#6880,#6881));
#2097=EDGE_LOOP('',(#6882,#6883,#6884,#6885,#6886,#6887,#6888,#6889));
#2098=EDGE_LOOP('',(#6890,#6891,#6892,#6893,#6894,#6895,#6896,#6897,#6898,
#6899,#6900,#6901));
#2099=EDGE_LOOP('',(#6902,#6903,#6904,#6905,#6906,#6907,#6908,#6909,#6910,
#6911,#6912,#6913));
#2100=EDGE_LOOP('',(#6914,#6915,#6916,#6917,#6918,#6919,#6920,#6921,#6922,
#6923,#6924,#6925));
#2101=EDGE_LOOP('',(#6926,#6927,#6928,#6929,#6930,#6931,#6932,#6933,#6934,
#6935));
#2102=EDGE_LOOP('',(#6936,#6937,#6938,#6939));
#2103=EDGE_LOOP('',(#6940,#6941,#6942,#6943));
#2104=EDGE_LOOP('',(#6944));
#2105=EDGE_LOOP('',(#6945));
#2106=EDGE_LOOP('',(#6946));
#2107=EDGE_LOOP('',(#6947));
#2108=EDGE_LOOP('',(#6948,#6949,#6950,#6951));
#2109=EDGE_LOOP('',(#6952,#6953,#6954,#6955,#6956,#6957,#6958,#6959,#6960,
#6961));
#2110=EDGE_LOOP('',(#6962,#6963,#6964,#6965));
#2111=EDGE_LOOP('',(#6966,#6967,#6968,#6969));
#2112=EDGE_LOOP('',(#6970,#6971,#6972,#6973));
#2113=EDGE_LOOP('',(#6974,#6975,#6976,#6977));
#2114=EDGE_LOOP('',(#6978,#6979,#6980,#6981));
#2115=EDGE_LOOP('',(#6982,#6983,#6984,#6985,#6986,#6987,#6988,#6989,#6990,
#6991,#6992,#6993));
#2116=EDGE_LOOP('',(#6994,#6995,#6996,#6997));
#2117=EDGE_LOOP('',(#6998,#6999,#7000,#7001));
#2118=EDGE_LOOP('',(#7002,#7003,#7004,#7005));
#2119=EDGE_LOOP('',(#7006,#7007,#7008,#7009));
#2120=EDGE_LOOP('',(#7010,#7011,#7012,#7013));
#2121=EDGE_LOOP('',(#7014,#7015,#7016,#7017));
#2122=EDGE_LOOP('',(#7018,#7019,#7020,#7021));
#2123=EDGE_LOOP('',(#7022,#7023,#7024,#7025));
#2124=EDGE_LOOP('',(#7026,#7027,#7028,#7029,#7030,#7031,#7032,#7033));
#2125=EDGE_LOOP('',(#7034,#7035,#7036,#7037,#7038,#7039,#7040,#7041));
#2126=EDGE_LOOP('',(#7042,#7043,#7044,#7045));
#2127=EDGE_LOOP('',(#7046,#7047,#7048,#7049));
#2128=EDGE_LOOP('',(#7050,#7051,#7052,#7053));
#2129=EDGE_LOOP('',(#7054,#7055,#7056,#7057));
#2130=EDGE_LOOP('',(#7058,#7059,#7060,#7061));
#2131=EDGE_LOOP('',(#7062,#7063,#7064,#7065));
#2132=EDGE_LOOP('',(#7066,#7067,#7068,#7069));
#2133=EDGE_LOOP('',(#7070,#7071,#7072,#7073));
#2134=EDGE_LOOP('',(#7074,#7075,#7076,#7077,#7078,#7079,#7080,#7081));
#2135=EDGE_LOOP('',(#7082,#7083,#7084,#7085,#7086,#7087,#7088,#7089));
#2136=EDGE_LOOP('',(#7090,#7091,#7092,#7093));
#2137=EDGE_LOOP('',(#7094,#7095,#7096,#7097));
#2138=EDGE_LOOP('',(#7098,#7099,#7100,#7101));
#2139=EDGE_LOOP('',(#7102,#7103,#7104,#7105));
#2140=EDGE_LOOP('',(#7106,#7107,#7108,#7109));
#2141=EDGE_LOOP('',(#7110,#7111,#7112,#7113));
#2142=EDGE_LOOP('',(#7114,#7115,#7116,#7117,#7118,#7119));
#2143=EDGE_LOOP('',(#7120,#7121,#7122,#7123,#7124,#7125));
#2144=EDGE_LOOP('',(#7126));
#2145=EDGE_LOOP('',(#7127));
#2146=EDGE_LOOP('',(#7128,#7129,#7130,#7131));
#2147=EDGE_LOOP('',(#7132,#7133,#7134,#7135));
#2148=EDGE_LOOP('',(#7136,#7137,#7138,#7139));
#2149=EDGE_LOOP('',(#7140));
#2150=EDGE_LOOP('',(#7141));
#2151=EDGE_LOOP('',(#7142,#7143,#7144,#7145));
#2152=EDGE_LOOP('',(#7146,#7147,#7148,#7149));
#2153=EDGE_LOOP('',(#7150,#7151,#7152,#7153));
#2154=EDGE_LOOP('',(#7154,#7155,#7156,#7157));
#2155=EDGE_LOOP('',(#7158,#7159,#7160,#7161));
#2156=EDGE_LOOP('',(#7162,#7163,#7164,#7165));
#2157=EDGE_LOOP('',(#7166,#7167,#7168,#7169));
#2158=EDGE_LOOP('',(#7170,#7171,#7172,#7173));
#2159=EDGE_LOOP('',(#7174,#7175,#7176,#7177,#7178,#7179));
#2160=EDGE_LOOP('',(#7180,#7181,#7182,#7183,#7184,#7185));
#2161=EDGE_LOOP('',(#7186));
#2162=EDGE_LOOP('',(#7187));
#2163=EDGE_LOOP('',(#7188,#7189,#7190,#7191));
#2164=EDGE_LOOP('',(#7192,#7193,#7194,#7195));
#2165=EDGE_LOOP('',(#7196,#7197,#7198,#7199));
#2166=EDGE_LOOP('',(#7200));
#2167=EDGE_LOOP('',(#7201));
#2168=EDGE_LOOP('',(#7202,#7203,#7204,#7205));
#2169=EDGE_LOOP('',(#7206,#7207,#7208,#7209));
#2170=LINE('',#11953,#2693);
#2171=LINE('',#11959,#2694);
#2172=LINE('',#11965,#2695);
#2173=LINE('',#11971,#2696);
#2174=LINE('',#11977,#2697);
#2175=LINE('',#11983,#2698);
#2176=LINE('',#11989,#2699);
#2177=LINE('',#11995,#2700);
#2178=LINE('',#12001,#2701);
#2179=LINE('',#12007,#2702);
#2180=LINE('',#12013,#2703);
#2181=LINE('',#12019,#2704);
#2182=LINE('',#12024,#2705);
#2183=LINE('',#12026,#2706);
#2184=LINE('',#12028,#2707);
#2185=LINE('',#12029,#2708);
#2186=LINE('',#12032,#2709);
#2187=LINE('',#12034,#2710);
#2188=LINE('',#12035,#2711);
#2189=LINE('',#12038,#2712);
#2190=LINE('',#12040,#2713);
#2191=LINE('',#12041,#2714);
#2192=LINE('',#12043,#2715);
#2193=LINE('',#12044,#2716);
#2194=LINE('',#12051,#2717);
#2195=LINE('',#12053,#2718);
#2196=LINE('',#12055,#2719);
#2197=LINE('',#12056,#2720);
#2198=LINE('',#12059,#2721);
#2199=LINE('',#12061,#2722);
#2200=LINE('',#12062,#2723);
#2201=LINE('',#12065,#2724);
#2202=LINE('',#12067,#2725);
#2203=LINE('',#12068,#2726);
#2204=LINE('',#12070,#2727);
#2205=LINE('',#12071,#2728);
#2206=LINE('',#12078,#2729);
#2207=LINE('',#12080,#2730);
#2208=LINE('',#12082,#2731);
#2209=LINE('',#12083,#2732);
#2210=LINE('',#12086,#2733);
#2211=LINE('',#12088,#2734);
#2212=LINE('',#12089,#2735);
#2213=LINE('',#12092,#2736);
#2214=LINE('',#12094,#2737);
#2215=LINE('',#12095,#2738);
#2216=LINE('',#12097,#2739);
#2217=LINE('',#12098,#2740);
#2218=LINE('',#12142,#2741);
#2219=LINE('',#12184,#2742);
#2220=LINE('',#12191,#2743);
#2221=LINE('',#12198,#2744);
#2222=LINE('',#12205,#2745);
#2223=LINE('',#12211,#2746);
#2224=LINE('',#12215,#2747);
#2225=LINE('',#12222,#2748);
#2226=LINE('',#12226,#2749);
#2227=LINE('',#12233,#2750);
#2228=LINE('',#12237,#2751);
#2229=LINE('',#12244,#2752);
#2230=LINE('',#12248,#2753);
#2231=LINE('',#12272,#2754);
#2232=LINE('',#12276,#2755);
#2233=LINE('',#12280,#2756);
#2234=LINE('',#12284,#2757);
#2235=LINE('',#12288,#2758);
#2236=LINE('',#12293,#2759);
#2237=LINE('',#12300,#2760);
#2238=LINE('',#12304,#2761);
#2239=LINE('',#12313,#2762);
#2240=LINE('',#12322,#2763);
#2241=LINE('',#12331,#2764);
#2242=LINE('',#12340,#2765);
#2243=LINE('',#12348,#2766);
#2244=LINE('',#12352,#2767);
#2245=LINE('',#12356,#2768);
#2246=LINE('',#12360,#2769);
#2247=LINE('',#12365,#2770);
#2248=LINE('',#12373,#2771);
#2249=LINE('',#12378,#2772);
#2250=LINE('',#12423,#2773);
#2251=LINE('',#12465,#2774);
#2252=LINE('',#12472,#2775);
#2253=LINE('',#12479,#2776);
#2254=LINE('',#12486,#2777);
#2255=LINE('',#12492,#2778);
#2256=LINE('',#12496,#2779);
#2257=LINE('',#12503,#2780);
#2258=LINE('',#12507,#2781);
#2259=LINE('',#12514,#2782);
#2260=LINE('',#12518,#2783);
#2261=LINE('',#12525,#2784);
#2262=LINE('',#12529,#2785);
#2263=LINE('',#12553,#2786);
#2264=LINE('',#12557,#2787);
#2265=LINE('',#12561,#2788);
#2266=LINE('',#12565,#2789);
#2267=LINE('',#12569,#2790);
#2268=LINE('',#12574,#2791);
#2269=LINE('',#12581,#2792);
#2270=LINE('',#12585,#2793);
#2271=LINE('',#12594,#2794);
#2272=LINE('',#12603,#2795);
#2273=LINE('',#12612,#2796);
#2274=LINE('',#12621,#2797);
#2275=LINE('',#12629,#2798);
#2276=LINE('',#12633,#2799);
#2277=LINE('',#12637,#2800);
#2278=LINE('',#12641,#2801);
#2279=LINE('',#12646,#2802);
#2280=LINE('',#12654,#2803);
#2281=LINE('',#12659,#2804);
#2282=LINE('',#12668,#2805);
#2283=LINE('',#12677,#2806);
#2284=LINE('',#12686,#2807);
#2285=LINE('',#12695,#2808);
#2286=LINE('',#12703,#2809);
#2287=LINE('',#12707,#2810);
#2288=LINE('',#12711,#2811);
#2289=LINE('',#12715,#2812);
#2290=LINE('',#12719,#2813);
#2291=LINE('',#12721,#2814);
#2292=LINE('',#12723,#2815);
#2293=LINE('',#12724,#2816);
#2294=LINE('',#12727,#2817);
#2295=LINE('',#12729,#2818);
#2296=LINE('',#12730,#2819);
#2297=LINE('',#12733,#2820);
#2298=LINE('',#12735,#2821);
#2299=LINE('',#12736,#2822);
#2300=LINE('',#12739,#2823);
#2301=LINE('',#12741,#2824);
#2302=LINE('',#12742,#2825);
#2303=LINE('',#12745,#2826);
#2304=LINE('',#12747,#2827);
#2305=LINE('',#12748,#2828);
#2306=LINE('',#12751,#2829);
#2307=LINE('',#12753,#2830);
#2308=LINE('',#12754,#2831);
#2309=LINE('',#12757,#2832);
#2310=LINE('',#12759,#2833);
#2311=LINE('',#12760,#2834);
#2312=LINE('',#12763,#2835);
#2313=LINE('',#12765,#2836);
#2314=LINE('',#12766,#2837);
#2315=LINE('',#12769,#2838);
#2316=LINE('',#12771,#2839);
#2317=LINE('',#12772,#2840);
#2318=LINE('',#12775,#2841);
#2319=LINE('',#12777,#2842);
#2320=LINE('',#12778,#2843);
#2321=LINE('',#12781,#2844);
#2322=LINE('',#12783,#2845);
#2323=LINE('',#12784,#2846);
#2324=LINE('',#12786,#2847);
#2325=LINE('',#12787,#2848);
#2326=LINE('',#12804,#2849);
#2327=LINE('',#12810,#2850);
#2328=LINE('',#12814,#2851);
#2329=LINE('',#12820,#2852);
#2330=LINE('',#12825,#2853);
#2331=LINE('',#12840,#2854);
#2332=LINE('',#12849,#2855);
#2333=LINE('',#12853,#2856);
#2334=LINE('',#12857,#2857);
#2335=LINE('',#12860,#2858);
#2336=LINE('',#13013,#2859);
#2337=LINE('',#13309,#2860);
#2338=LINE('',#13351,#2861);
#2339=LINE('',#13356,#2862);
#2340=LINE('',#13365,#2863);
#2341=LINE('',#13370,#2864);
#2342=LINE('',#13382,#2865);
#2343=LINE('',#13387,#2866);
#2344=LINE('',#13391,#2867);
#2345=LINE('',#13395,#2868);
#2346=LINE('',#13397,#2869);
#2347=LINE('',#13398,#2870);
#2348=LINE('',#13401,#2871);
#2349=LINE('',#13405,#2872);
#2350=LINE('',#13409,#2873);
#2351=LINE('',#13417,#2874);
#2352=LINE('',#13418,#2875);
#2353=LINE('',#13422,#2876);
#2354=LINE('',#13425,#2877);
#2355=LINE('',#13429,#2878);
#2356=LINE('',#13431,#2879);
#2357=LINE('',#13435,#2880);
#2358=LINE('',#13436,#2881);
#2359=LINE('',#13439,#2882);
#2360=LINE('',#13448,#2883);
#2361=LINE('',#13451,#2884);
#2362=LINE('',#13459,#2885);
#2363=LINE('',#13466,#2886);
#2364=LINE('',#13475,#2887);
#2365=LINE('',#13481,#2888);
#2366=LINE('',#13489,#2889);
#2367=LINE('',#13519,#2890);
#2368=LINE('',#13566,#2891);
#2369=LINE('',#13571,#2892);
#2370=LINE('',#13577,#2893);
#2371=LINE('',#13586,#2894);
#2372=LINE('',#13600,#2895);
#2373=LINE('',#13603,#2896);
#2374=LINE('',#13608,#2897);
#2375=LINE('',#13616,#2898);
#2376=LINE('',#13622,#2899);
#2377=LINE('',#13631,#2900);
#2378=LINE('',#13637,#2901);
#2379=LINE('',#13646,#2902);
#2380=LINE('',#13652,#2903);
#2381=LINE('',#13663,#2904);
#2382=LINE('',#13667,#2905);
#2383=LINE('',#13671,#2906);
#2384=LINE('',#13678,#2907);
#2385=LINE('',#13682,#2908);
#2386=LINE('',#13686,#2909);
#2387=LINE('',#13691,#2910);
#2388=LINE('',#13693,#2911);
#2389=LINE('',#13695,#2912);
#2390=LINE('',#13696,#2913);
#2391=LINE('',#13699,#2914);
#2392=LINE('',#13701,#2915);
#2393=LINE('',#13702,#2916);
#2394=LINE('',#13705,#2917);
#2395=LINE('',#13707,#2918);
#2396=LINE('',#13708,#2919);
#2397=LINE('',#13711,#2920);
#2398=LINE('',#13713,#2921);
#2399=LINE('',#13714,#2922);
#2400=LINE('',#13717,#2923);
#2401=LINE('',#13719,#2924);
#2402=LINE('',#13720,#2925);
#2403=LINE('',#13722,#2926);
#2404=LINE('',#13723,#2927);
#2405=LINE('',#13732,#2928);
#2406=LINE('',#13737,#2929);
#2407=LINE('',#13739,#2930);
#2408=LINE('',#13741,#2931);
#2409=LINE('',#13742,#2932);
#2410=LINE('',#13745,#2933);
#2411=LINE('',#13747,#2934);
#2412=LINE('',#13748,#2935);
#2413=LINE('',#13751,#2936);
#2414=LINE('',#13753,#2937);
#2415=LINE('',#13754,#2938);
#2416=LINE('',#13756,#2939);
#2417=LINE('',#13757,#2940);
#2418=LINE('',#13761,#2941);
#2419=LINE('',#13765,#2942);
#2420=LINE('',#13769,#2943);
#2421=LINE('',#13772,#2944);
#2422=LINE('',#13777,#2945);
#2423=LINE('',#13778,#2946);
#2424=LINE('',#13781,#2947);
#2425=LINE('',#13782,#2948);
#2426=LINE('',#13791,#2949);
#2427=LINE('',#13794,#2950);
#2428=LINE('',#13803,#2951);
#2429=LINE('',#13809,#2952);
#2430=LINE('',#13817,#2953);
#2431=LINE('',#13847,#2954);
#2432=LINE('',#13894,#2955);
#2433=LINE('',#13899,#2956);
#2434=LINE('',#13905,#2957);
#2435=LINE('',#13914,#2958);
#2436=LINE('',#13928,#2959);
#2437=LINE('',#13931,#2960);
#2438=LINE('',#13936,#2961);
#2439=LINE('',#13944,#2962);
#2440=LINE('',#13950,#2963);
#2441=LINE('',#13959,#2964);
#2442=LINE('',#13965,#2965);
#2443=LINE('',#13974,#2966);
#2444=LINE('',#13980,#2967);
#2445=LINE('',#13991,#2968);
#2446=LINE('',#13993,#2969);
#2447=LINE('',#13995,#2970);
#2448=LINE('',#13996,#2971);
#2449=LINE('',#13999,#2972);
#2450=LINE('',#14001,#2973);
#2451=LINE('',#14002,#2974);
#2452=LINE('',#14005,#2975);
#2453=LINE('',#14007,#2976);
#2454=LINE('',#14008,#2977);
#2455=LINE('',#14011,#2978);
#2456=LINE('',#14013,#2979);
#2457=LINE('',#14014,#2980);
#2458=LINE('',#14017,#2981);
#2459=LINE('',#14019,#2982);
#2460=LINE('',#14020,#2983);
#2461=LINE('',#14022,#2984);
#2462=LINE('',#14023,#2985);
#2463=LINE('',#14031,#2986);
#2464=LINE('',#14033,#2987);
#2465=LINE('',#14040,#2988);
#2466=LINE('',#14045,#2989);
#2467=LINE('',#14047,#2990);
#2468=LINE('',#14049,#2991);
#2469=LINE('',#14050,#2992);
#2470=LINE('',#14054,#2993);
#2471=LINE('',#14056,#2994);
#2472=LINE('',#14058,#2995);
#2473=LINE('',#14059,#2996);
#2474=LINE('',#14062,#2997);
#2475=LINE('',#14064,#2998);
#2476=LINE('',#14065,#2999);
#2477=LINE('',#14068,#3000);
#2478=LINE('',#14070,#3001);
#2479=LINE('',#14071,#3002);
#2480=LINE('',#14073,#3003);
#2481=LINE('',#14074,#3004);
#2482=LINE('',#14078,#3005);
#2483=LINE('',#14080,#3006);
#2484=LINE('',#14082,#3007);
#2485=LINE('',#14083,#3008);
#2486=LINE('',#14087,#3009);
#2487=LINE('',#14089,#3010);
#2488=LINE('',#14091,#3011);
#2489=LINE('',#14092,#3012);
#2490=LINE('',#14096,#3013);
#2491=LINE('',#14097,#3014);
#2492=LINE('',#14098,#3015);
#2493=LINE('',#14102,#3016);
#2494=LINE('',#14103,#3017);
#2495=LINE('',#14104,#3018);
#2496=LINE('',#14106,#3019);
#2497=LINE('',#14107,#3020);
#2498=LINE('',#14109,#3021);
#2499=LINE('',#14110,#3022);
#2500=LINE('',#14112,#3023);
#2501=LINE('',#14114,#3024);
#2502=LINE('',#14123,#3025);
#2503=LINE('',#14129,#3026);
#2504=LINE('',#14134,#3027);
#2505=LINE('',#14138,#3028);
#2506=LINE('',#14142,#3029);
#2507=LINE('',#14144,#3030);
#2508=LINE('',#14145,#3031);
#2509=LINE('',#14148,#3032);
#2510=LINE('',#14152,#3033);
#2511=LINE('',#14153,#3034);
#2512=LINE('',#14162,#3035);
#2513=LINE('',#14168,#3036);
#2514=LINE('',#14177,#3037);
#2515=LINE('',#14183,#3038);
#2516=LINE('',#14196,#3039);
#2517=LINE('',#14202,#3040);
#2518=LINE('',#14208,#3041);
#2519=LINE('',#14214,#3042);
#2520=LINE('',#14220,#3043);
#2521=LINE('',#14225,#3044);
#2522=LINE('',#14227,#3045);
#2523=LINE('',#14229,#3046);
#2524=LINE('',#14230,#3047);
#2525=LINE('',#14233,#3048);
#2526=LINE('',#14235,#3049);
#2527=LINE('',#14236,#3050);
#2528=LINE('',#14239,#3051);
#2529=LINE('',#14241,#3052);
#2530=LINE('',#14242,#3053);
#2531=LINE('',#14244,#3054);
#2532=LINE('',#14245,#3055);
#2533=LINE('',#14253,#3056);
#2534=LINE('',#14267,#3057);
#2535=LINE('',#14270,#3058);
#2536=LINE('',#14275,#3059);
#2537=LINE('',#14283,#3060);
#2538=LINE('',#14289,#3061);
#2539=LINE('',#14298,#3062);
#2540=LINE('',#14304,#3063);
#2541=LINE('',#14313,#3064);
#2542=LINE('',#14319,#3065);
#2543=LINE('',#14328,#3066);
#2544=LINE('',#14332,#3067);
#2545=LINE('',#14336,#3068);
#2546=LINE('',#14340,#3069);
#2547=LINE('',#14344,#3070);
#2548=LINE('',#14348,#3071);
#2549=LINE('',#14352,#3072);
#2550=LINE('',#14356,#3073);
#2551=LINE('',#14360,#3074);
#2552=LINE('',#14364,#3075);
#2553=LINE('',#14368,#3076);
#2554=LINE('',#14372,#3077);
#2555=LINE('',#14376,#3078);
#2556=LINE('',#14380,#3079);
#2557=LINE('',#14384,#3080);
#2558=LINE('',#14388,#3081);
#2559=LINE('',#14390,#3082);
#2560=LINE('',#14392,#3083);
#2561=LINE('',#14394,#3084);
#2562=LINE('',#14396,#3085);
#2563=LINE('',#14398,#3086);
#2564=LINE('',#14399,#3087);
#2565=LINE('',#14401,#3088);
#2566=LINE('',#14403,#3089);
#2567=LINE('',#14405,#3090);
#2568=LINE('',#14407,#3091);
#2569=LINE('',#14409,#3092);
#2570=LINE('',#14410,#3093);
#2571=LINE('',#14413,#3094);
#2572=LINE('',#14415,#3095);
#2573=LINE('',#14417,#3096);
#2574=LINE('',#14419,#3097);
#2575=LINE('',#14420,#3098);
#2576=LINE('',#14422,#3099);
#2577=LINE('',#14424,#3100);
#2578=LINE('',#14426,#3101);
#2579=LINE('',#14428,#3102);
#2580=LINE('',#14429,#3103);
#2581=LINE('',#14432,#3104);
#2582=LINE('',#14433,#3105);
#2583=LINE('',#14436,#3106);
#2584=LINE('',#14437,#3107);
#2585=LINE('',#14440,#3108);
#2586=LINE('',#14441,#3109);
#2587=LINE('',#14444,#3110);
#2588=LINE('',#14445,#3111);
#2589=LINE('',#14447,#3112);
#2590=LINE('',#14450,#3113);
#2591=LINE('',#14451,#3114);
#2592=LINE('',#14454,#3115);
#2593=LINE('',#14455,#3116);
#2594=LINE('',#14458,#3117);
#2595=LINE('',#14459,#3118);
#2596=LINE('',#14462,#3119);
#2597=LINE('',#14463,#3120);
#2598=LINE('',#14465,#3121);
#2599=LINE('',#14471,#3122);
#2600=LINE('',#14473,#3123);
#2601=LINE('',#14475,#3124);
#2602=LINE('',#14476,#3125);
#2603=LINE('',#14479,#3126);
#2604=LINE('',#14481,#3127);
#2605=LINE('',#14482,#3128);
#2606=LINE('',#14485,#3129);
#2607=LINE('',#14487,#3130);
#2608=LINE('',#14488,#3131);
#2609=LINE('',#14491,#3132);
#2610=LINE('',#14493,#3133);
#2611=LINE('',#14494,#3134);
#2612=LINE('',#14497,#3135);
#2613=LINE('',#14499,#3136);
#2614=LINE('',#14500,#3137);
#2615=LINE('',#14503,#3138);
#2616=LINE('',#14505,#3139);
#2617=LINE('',#14506,#3140);
#2618=LINE('',#14509,#3141);
#2619=LINE('',#14511,#3142);
#2620=LINE('',#14512,#3143);
#2621=LINE('',#14514,#3144);
#2622=LINE('',#14515,#3145);
#2623=LINE('',#14522,#3146);
#2624=LINE('',#14524,#3147);
#2625=LINE('',#14526,#3148);
#2626=LINE('',#14527,#3149);
#2627=LINE('',#14530,#3150);
#2628=LINE('',#14532,#3151);
#2629=LINE('',#14533,#3152);
#2630=LINE('',#14536,#3153);
#2631=LINE('',#14538,#3154);
#2632=LINE('',#14539,#3155);
#2633=LINE('',#14542,#3156);
#2634=LINE('',#14544,#3157);
#2635=LINE('',#14545,#3158);
#2636=LINE('',#14548,#3159);
#2637=LINE('',#14550,#3160);
#2638=LINE('',#14551,#3161);
#2639=LINE('',#14554,#3162);
#2640=LINE('',#14556,#3163);
#2641=LINE('',#14557,#3164);
#2642=LINE('',#14560,#3165);
#2643=LINE('',#14562,#3166);
#2644=LINE('',#14563,#3167);
#2645=LINE('',#14565,#3168);
#2646=LINE('',#14566,#3169);
#2647=LINE('',#14576,#3170);
#2648=LINE('',#14578,#3171);
#2649=LINE('',#14580,#3172);
#2650=LINE('',#14581,#3173);
#2651=LINE('',#14584,#3174);
#2652=LINE('',#14586,#3175);
#2653=LINE('',#14587,#3176);
#2654=LINE('',#14590,#3177);
#2655=LINE('',#14592,#3178);
#2656=LINE('',#14593,#3179);
#2657=LINE('',#14596,#3180);
#2658=LINE('',#14598,#3181);
#2659=LINE('',#14599,#3182);
#2660=LINE('',#14602,#3183);
#2661=LINE('',#14604,#3184);
#2662=LINE('',#14605,#3185);
#2663=LINE('',#14607,#3186);
#2664=LINE('',#14608,#3187);
#2665=LINE('',#14620,#3188);
#2666=LINE('',#14624,#3189);
#2667=LINE('',#14628,#3190);
#2668=LINE('',#14635,#3191);
#2669=LINE('',#14637,#3192);
#2670=LINE('',#14642,#3193);
#2671=LINE('',#14644,#3194);
#2672=LINE('',#14646,#3195);
#2673=LINE('',#14647,#3196);
#2674=LINE('',#14650,#3197);
#2675=LINE('',#14652,#3198);
#2676=LINE('',#14653,#3199);
#2677=LINE('',#14656,#3200);
#2678=LINE('',#14658,#3201);
#2679=LINE('',#14659,#3202);
#2680=LINE('',#14662,#3203);
#2681=LINE('',#14664,#3204);
#2682=LINE('',#14665,#3205);
#2683=LINE('',#14668,#3206);
#2684=LINE('',#14670,#3207);
#2685=LINE('',#14671,#3208);
#2686=LINE('',#14673,#3209);
#2687=LINE('',#14674,#3210);
#2688=LINE('',#14686,#3211);
#2689=LINE('',#14690,#3212);
#2690=LINE('',#14694,#3213);
#2691=LINE('',#14701,#3214);
#2692=LINE('',#14703,#3215);
#2693=VECTOR('',#9407,0.21);
#2694=VECTOR('',#9414,0.21);
#2695=VECTOR('',#9421,0.21);
#2696=VECTOR('',#9428,0.21);
#2697=VECTOR('',#9435,0.21);
#2698=VECTOR('',#9442,0.21);
#2699=VECTOR('',#9449,0.21);
#2700=VECTOR('',#9456,0.21);
#2701=VECTOR('',#9463,0.164999999999999);
#2702=VECTOR('',#9470,0.164999999999999);
#2703=VECTOR('',#9477,0.165);
#2704=VECTOR('',#9484,0.165);
#2705=VECTOR('',#9489,1.);
#2706=VECTOR('',#9490,1.);
#2707=VECTOR('',#9491,1.);
#2708=VECTOR('',#9492,1.);
#2709=VECTOR('',#9495,1.);
#2710=VECTOR('',#9496,1.);
#2711=VECTOR('',#9497,1.);
#2712=VECTOR('',#9500,1.);
#2713=VECTOR('',#9501,1.);
#2714=VECTOR('',#9502,1.);
#2715=VECTOR('',#9505,1.);
#2716=VECTOR('',#9506,1.);
#2717=VECTOR('',#9515,1.);
#2718=VECTOR('',#9516,1.);
#2719=VECTOR('',#9517,1.);
#2720=VECTOR('',#9518,1.);
#2721=VECTOR('',#9521,1.);
#2722=VECTOR('',#9522,1.);
#2723=VECTOR('',#9523,1.);
#2724=VECTOR('',#9526,1.);
#2725=VECTOR('',#9527,1.);
#2726=VECTOR('',#9528,1.);
#2727=VECTOR('',#9531,1.);
#2728=VECTOR('',#9532,1.);
#2729=VECTOR('',#9541,1.);
#2730=VECTOR('',#9542,1.);
#2731=VECTOR('',#9543,1.);
#2732=VECTOR('',#9544,1.);
#2733=VECTOR('',#9547,1.);
#2734=VECTOR('',#9548,1.);
#2735=VECTOR('',#9549,1.);
#2736=VECTOR('',#9552,1.);
#2737=VECTOR('',#9553,1.);
#2738=VECTOR('',#9554,1.);
#2739=VECTOR('',#9557,1.);
#2740=VECTOR('',#9558,1.);
#2741=VECTOR('',#9567,0.25);
#2742=VECTOR('',#9572,0.165);
#2743=VECTOR('',#9581,0.165);
#2744=VECTOR('',#9590,0.165);
#2745=VECTOR('',#9599,0.165);
#2746=VECTOR('',#9606,1.);
#2747=VECTOR('',#9609,1.);
#2748=VECTOR('',#9618,1.);
#2749=VECTOR('',#9621,1.);
#2750=VECTOR('',#9630,1.);
#2751=VECTOR('',#9633,1.);
#2752=VECTOR('',#9642,1.);
#2753=VECTOR('',#9645,1.);
#2754=VECTOR('',#9678,0.275);
#2755=VECTOR('',#9683,0.275);
#2756=VECTOR('',#9688,0.275);
#2757=VECTOR('',#9693,0.275);
#2758=VECTOR('',#9698,2.2);
#2759=VECTOR('',#9703,1.5);
#2760=VECTOR('',#9712,2.9);
#2761=VECTOR('',#9717,1.02);
#2762=VECTOR('',#9730,0.375);
#2763=VECTOR('',#9741,0.375);
#2764=VECTOR('',#9752,0.375);
#2765=VECTOR('',#9763,0.375);
#2766=VECTOR('',#9774,0.225);
#2767=VECTOR('',#9779,0.225);
#2768=VECTOR('',#9784,0.225);
#2769=VECTOR('',#9789,0.225);
#2770=VECTOR('',#9794,1.49);
#2771=VECTOR('',#9805,0.71);
#2772=VECTOR('',#9810,2.2);
#2773=VECTOR('',#9821,0.25);
#2774=VECTOR('',#9826,0.165);
#2775=VECTOR('',#9835,0.165);
#2776=VECTOR('',#9844,0.165);
#2777=VECTOR('',#9853,0.165);
#2778=VECTOR('',#9860,1.);
#2779=VECTOR('',#9863,1.);
#2780=VECTOR('',#9872,1.);
#2781=VECTOR('',#9875,1.);
#2782=VECTOR('',#9884,1.);
#2783=VECTOR('',#9887,1.);
#2784=VECTOR('',#9896,1.);
#2785=VECTOR('',#9899,1.);
#2786=VECTOR('',#9932,0.275);
#2787=VECTOR('',#9937,0.275);
#2788=VECTOR('',#9942,0.275);
#2789=VECTOR('',#9947,0.275);
#2790=VECTOR('',#9952,2.2);
#2791=VECTOR('',#9957,1.5);
#2792=VECTOR('',#9966,2.9);
#2793=VECTOR('',#9971,1.02);
#2794=VECTOR('',#9984,0.375);
#2795=VECTOR('',#9995,0.375);
#2796=VECTOR('',#10006,0.375);
#2797=VECTOR('',#10017,0.375);
#2798=VECTOR('',#10028,0.225);
#2799=VECTOR('',#10033,0.225);
#2800=VECTOR('',#10038,0.225);
#2801=VECTOR('',#10043,0.225);
#2802=VECTOR('',#10048,1.49);
#2803=VECTOR('',#10059,0.71);
#2804=VECTOR('',#10064,2.2);
#2805=VECTOR('',#10077,0.375);
#2806=VECTOR('',#10088,0.375);
#2807=VECTOR('',#10099,0.375);
#2808=VECTOR('',#10110,0.375);
#2809=VECTOR('',#10121,0.225);
#2810=VECTOR('',#10126,0.225);
#2811=VECTOR('',#10131,0.225);
#2812=VECTOR('',#10136,0.225000000000001);
#2813=VECTOR('',#10139,1.);
#2814=VECTOR('',#10140,1.);
#2815=VECTOR('',#10141,1.);
#2816=VECTOR('',#10142,1.);
#2817=VECTOR('',#10145,1.);
#2818=VECTOR('',#10146,1.);
#2819=VECTOR('',#10147,1.);
#2820=VECTOR('',#10150,1.);
#2821=VECTOR('',#10151,1.);
#2822=VECTOR('',#10152,1.);
#2823=VECTOR('',#10155,1.);
#2824=VECTOR('',#10156,1.);
#2825=VECTOR('',#10157,1.);
#2826=VECTOR('',#10160,1.);
#2827=VECTOR('',#10161,1.);
#2828=VECTOR('',#10162,1.);
#2829=VECTOR('',#10165,1.);
#2830=VECTOR('',#10166,1.);
#2831=VECTOR('',#10167,1.);
#2832=VECTOR('',#10170,1.);
#2833=VECTOR('',#10171,1.);
#2834=VECTOR('',#10172,1.);
#2835=VECTOR('',#10175,1.);
#2836=VECTOR('',#10176,1.);
#2837=VECTOR('',#10177,1.);
#2838=VECTOR('',#10180,1.);
#2839=VECTOR('',#10181,1.);
#2840=VECTOR('',#10182,1.);
#2841=VECTOR('',#10185,1.);
#2842=VECTOR('',#10186,1.);
#2843=VECTOR('',#10187,1.);
#2844=VECTOR('',#10190,1.);
#2845=VECTOR('',#10191,1.);
#2846=VECTOR('',#10192,1.);
#2847=VECTOR('',#10195,1.);
#2848=VECTOR('',#10196,1.);
#2849=VECTOR('',#10219,0.976185);
#2850=VECTOR('',#10226,0.5);
#2851=VECTOR('',#10231,0.53);
#2852=VECTOR('',#10240,0.976185);
#2853=VECTOR('',#10247,0.53);
#2854=VECTOR('',#10266,1.023815);
#2855=VECTOR('',#10277,1.47);
#2856=VECTOR('',#10282,1.5);
#2857=VECTOR('',#10287,1.47);
#2858=VECTOR('',#10292,1.023815);
#2859=VECTOR('',#10343,1.019052);
#2860=VECTOR('',#10420,0.980948);
#2861=VECTOR('',#10449,1.013815);
#2862=VECTOR('',#10456,0.991185);
#2863=VECTOR('',#10467,1.013815);
#2864=VECTOR('',#10474,0.991185);
#2865=VECTOR('',#10493,0.225);
#2866=VECTOR('',#10498,1.);
#2867=VECTOR('',#10501,1.);
#2868=VECTOR('',#10506,1.);
#2869=VECTOR('',#10507,1.);
#2870=VECTOR('',#10508,1.);
#2871=VECTOR('',#10511,1.);
#2872=VECTOR('',#10514,1.);
#2873=VECTOR('',#10517,1.);
#2874=VECTOR('',#10526,1.);
#2875=VECTOR('',#10527,1.);
#2876=VECTOR('',#10532,1.);
#2877=VECTOR('',#10535,0.25);
#2878=VECTOR('',#10540,1.);
#2879=VECTOR('',#10541,1.);
#2880=VECTOR('',#10546,1.);
#2881=VECTOR('',#10547,1.);
#2882=VECTOR('',#10552,1.);
#2883=VECTOR('',#10565,0.7);
#2884=VECTOR('',#10568,0.5);
#2885=VECTOR('',#10579,0.165);
#2886=VECTOR('',#10588,0.6);
#2887=VECTOR('',#10601,0.505);
#2888=VECTOR('',#10608,0.7);
#2889=VECTOR('',#10619,1.);
#2890=VECTOR('',#10626,0.165);
#2891=VECTOR('',#10629,1.);
#2892=VECTOR('',#10634,0.505);
#2893=VECTOR('',#10641,0.9);
#2894=VECTOR('',#10654,0.165);
#2895=VECTOR('',#10673,0.7);
#2896=VECTOR('',#10676,0.3);
#2897=VECTOR('',#10683,0.3);
#2898=VECTOR('',#10694,0.305);
#2899=VECTOR('',#10701,0.5);
#2900=VECTOR('',#10714,0.305);
#2901=VECTOR('',#10721,0.5);
#2902=VECTOR('',#10734,0.225);
#2903=VECTOR('',#10741,0.5);
#2904=VECTOR('',#10758,0.325);
#2905=VECTOR('',#10763,0.35);
#2906=VECTOR('',#10768,0.335);
#2907=VECTOR('',#10777,0.21);
#2908=VECTOR('',#10782,0.2);
#2909=VECTOR('',#10787,0.18);
#2910=VECTOR('',#10792,1.);
#2911=VECTOR('',#10793,1.);
#2912=VECTOR('',#10794,1.);
#2913=VECTOR('',#10795,1.);
#2914=VECTOR('',#10798,1.);
#2915=VECTOR('',#10799,1.);
#2916=VECTOR('',#10800,1.);
#2917=VECTOR('',#10803,1.);
#2918=VECTOR('',#10804,1.);
#2919=VECTOR('',#10805,1.);
#2920=VECTOR('',#10808,1.);
#2921=VECTOR('',#10809,1.);
#2922=VECTOR('',#10810,1.);
#2923=VECTOR('',#10813,1.);
#2924=VECTOR('',#10814,1.);
#2925=VECTOR('',#10815,1.);
#2926=VECTOR('',#10818,1.);
#2927=VECTOR('',#10819,1.);
#2928=VECTOR('',#10832,0.25);
#2929=VECTOR('',#10837,1.);
#2930=VECTOR('',#10838,1.);
#2931=VECTOR('',#10839,1.);
#2932=VECTOR('',#10840,1.);
#2933=VECTOR('',#10843,1.);
#2934=VECTOR('',#10844,1.);
#2935=VECTOR('',#10845,1.);
#2936=VECTOR('',#10848,1.);
#2937=VECTOR('',#10849,1.);
#2938=VECTOR('',#10850,1.);
#2939=VECTOR('',#10853,1.);
#2940=VECTOR('',#10854,1.);
#2941=VECTOR('',#10857,1.);
#2942=VECTOR('',#10860,1.);
#2943=VECTOR('',#10865,1.);
#2944=VECTOR('',#10868,1.);
#2945=VECTOR('',#10873,1.);
#2946=VECTOR('',#10874,1.);
#2947=VECTOR('',#10877,1.);
#2948=VECTOR('',#10878,1.);
#2949=VECTOR('',#10891,0.7);
#2950=VECTOR('',#10894,0.5);
#2951=VECTOR('',#10907,0.505);
#2952=VECTOR('',#10914,0.7);
#2953=VECTOR('',#10925,1.);
#2954=VECTOR('',#10932,0.165);
#2955=VECTOR('',#10935,1.);
#2956=VECTOR('',#10940,0.505);
#2957=VECTOR('',#10947,0.9);
#2958=VECTOR('',#10960,0.165);
#2959=VECTOR('',#10979,0.7);
#2960=VECTOR('',#10982,0.3);
#2961=VECTOR('',#10989,0.3);
#2962=VECTOR('',#11000,0.305);
#2963=VECTOR('',#11007,0.5);
#2964=VECTOR('',#11020,0.305);
#2965=VECTOR('',#11027,0.5);
#2966=VECTOR('',#11040,0.225);
#2967=VECTOR('',#11047,0.5);
#2968=VECTOR('',#11062,1.);
#2969=VECTOR('',#11063,1.);
#2970=VECTOR('',#11064,1.);
#2971=VECTOR('',#11065,1.);
#2972=VECTOR('',#11068,1.);
#2973=VECTOR('',#11069,1.);
#2974=VECTOR('',#11070,1.);
#2975=VECTOR('',#11073,1.);
#2976=VECTOR('',#11074,1.);
#2977=VECTOR('',#11075,1.);
#2978=VECTOR('',#11078,1.);
#2979=VECTOR('',#11079,1.);
#2980=VECTOR('',#11080,1.);
#2981=VECTOR('',#11083,1.);
#2982=VECTOR('',#11084,1.);
#2983=VECTOR('',#11085,1.);
#2984=VECTOR('',#11088,1.);
#2985=VECTOR('',#11089,1.);
#2986=VECTOR('',#11100,0.185);
#2987=VECTOR('',#11103,0.2);
#2988=VECTOR('',#11112,0.305);
#2989=VECTOR('',#11117,1.);
#2990=VECTOR('',#11118,1.);
#2991=VECTOR('',#11119,1.);
#2992=VECTOR('',#11120,1.);
#2993=VECTOR('',#11123,1.);
#2994=VECTOR('',#11124,1.);
#2995=VECTOR('',#11125,1.);
#2996=VECTOR('',#11126,1.);
#2997=VECTOR('',#11129,1.);
#2998=VECTOR('',#11130,1.);
#2999=VECTOR('',#11131,1.);
#3000=VECTOR('',#11134,1.);
#3001=VECTOR('',#11135,1.);
#3002=VECTOR('',#11136,1.);
#3003=VECTOR('',#11139,1.);
#3004=VECTOR('',#11140,1.);
#3005=VECTOR('',#11143,1.);
#3006=VECTOR('',#11144,1.);
#3007=VECTOR('',#11145,1.);
#3008=VECTOR('',#11146,1.);
#3009=VECTOR('',#11149,1.);
#3010=VECTOR('',#11150,1.);
#3011=VECTOR('',#11151,1.);
#3012=VECTOR('',#11152,1.);
#3013=VECTOR('',#11155,1.);
#3014=VECTOR('',#11156,1.);
#3015=VECTOR('',#11157,1.);
#3016=VECTOR('',#11160,1.);
#3017=VECTOR('',#11161,1.);
#3018=VECTOR('',#11162,1.);
#3019=VECTOR('',#11165,1.);
#3020=VECTOR('',#11166,1.);
#3021=VECTOR('',#11169,1.);
#3022=VECTOR('',#11170,1.);
#3023=VECTOR('',#11173,1.);
#3024=VECTOR('',#11176,1.);
#3025=VECTOR('',#11189,0.5);
#3026=VECTOR('',#11196,0.5);
#3027=VECTOR('',#11201,1.);
#3028=VECTOR('',#11204,1.);
#3029=VECTOR('',#11209,1.);
#3030=VECTOR('',#11210,1.);
#3031=VECTOR('',#11211,1.);
#3032=VECTOR('',#11214,1.);
#3033=VECTOR('',#11219,1.);
#3034=VECTOR('',#11220,1.);
#3035=VECTOR('',#11233,0.305);
#3036=VECTOR('',#11240,0.5);
#3037=VECTOR('',#11253,0.305);
#3038=VECTOR('',#11260,0.5);
#3039=VECTOR('',#11281,0.25);
#3040=VECTOR('',#11288,0.275);
#3041=VECTOR('',#11295,0.275);
#3042=VECTOR('',#11302,0.275);
#3043=VECTOR('',#11309,0.275);
#3044=VECTOR('',#11314,1.);
#3045=VECTOR('',#11315,1.);
#3046=VECTOR('',#11316,1.);
#3047=VECTOR('',#11317,1.);
#3048=VECTOR('',#11320,1.);
#3049=VECTOR('',#11321,1.);
#3050=VECTOR('',#11322,1.);
#3051=VECTOR('',#11325,1.);
#3052=VECTOR('',#11326,1.);
#3053=VECTOR('',#11327,1.);
#3054=VECTOR('',#11330,1.);
#3055=VECTOR('',#11331,1.);
#3056=VECTOR('',#11342,0.164999999999999);
#3057=VECTOR('',#11361,0.699999999999999);
#3058=VECTOR('',#11364,0.300000000000001);
#3059=VECTOR('',#11371,0.300000000000001);
#3060=VECTOR('',#11382,0.305);
#3061=VECTOR('',#11389,0.5);
#3062=VECTOR('',#11402,0.305);
#3063=VECTOR('',#11409,0.5);
#3064=VECTOR('',#11422,0.225);
#3065=VECTOR('',#11429,0.5);
#3066=VECTOR('',#11442,1.);
#3067=VECTOR('',#11447,1.);
#3068=VECTOR('',#11450,0.21);
#3069=VECTOR('',#11455,1.);
#3070=VECTOR('',#11458,1.);
#3071=VECTOR('',#11463,1.);
#3072=VECTOR('',#11466,0.21);
#3073=VECTOR('',#11471,1.);
#3074=VECTOR('',#11474,1.);
#3075=VECTOR('',#11479,1.);
#3076=VECTOR('',#11482,0.21);
#3077=VECTOR('',#11487,1.);
#3078=VECTOR('',#11490,1.);
#3079=VECTOR('',#11495,1.);
#3080=VECTOR('',#11498,0.21);
#3081=VECTOR('',#11503,1.);
#3082=VECTOR('',#11506,1.);
#3083=VECTOR('',#11507,1.);
#3084=VECTOR('',#11508,1.);
#3085=VECTOR('',#11509,1.);
#3086=VECTOR('',#11510,1.);
#3087=VECTOR('',#11511,1.);
#3088=VECTOR('',#11514,1.);
#3089=VECTOR('',#11515,1.);
#3090=VECTOR('',#11516,1.);
#3091=VECTOR('',#11517,1.);
#3092=VECTOR('',#11518,1.);
#3093=VECTOR('',#11519,1.);
#3094=VECTOR('',#11522,1.);
#3095=VECTOR('',#11523,1.);
#3096=VECTOR('',#11524,1.);
#3097=VECTOR('',#11525,1.);
#3098=VECTOR('',#11526,1.);
#3099=VECTOR('',#11527,1.);
#3100=VECTOR('',#11528,1.);
#3101=VECTOR('',#11529,1.);
#3102=VECTOR('',#11530,1.);
#3103=VECTOR('',#11531,1.);
#3104=VECTOR('',#11534,1.);
#3105=VECTOR('',#11535,1.);
#3106=VECTOR('',#11538,1.);
#3107=VECTOR('',#11539,1.);
#3108=VECTOR('',#11542,1.);
#3109=VECTOR('',#11543,1.);
#3110=VECTOR('',#11546,1.);
#3111=VECTOR('',#11547,1.);
#3112=VECTOR('',#11550,1.);
#3113=VECTOR('',#11553,1.);
#3114=VECTOR('',#11554,1.);
#3115=VECTOR('',#11557,1.);
#3116=VECTOR('',#11558,1.);
#3117=VECTOR('',#11561,1.);
#3118=VECTOR('',#11562,1.);
#3119=VECTOR('',#11565,1.);
#3120=VECTOR('',#11566,1.);
#3121=VECTOR('',#11569,1.);
#3122=VECTOR('',#11576,1.);
#3123=VECTOR('',#11577,1.);
#3124=VECTOR('',#11578,1.);
#3125=VECTOR('',#11579,1.);
#3126=VECTOR('',#11582,1.);
#3127=VECTOR('',#11583,1.);
#3128=VECTOR('',#11584,1.);
#3129=VECTOR('',#11587,1.);
#3130=VECTOR('',#11588,1.);
#3131=VECTOR('',#11589,1.);
#3132=VECTOR('',#11592,1.);
#3133=VECTOR('',#11593,1.);
#3134=VECTOR('',#11594,1.);
#3135=VECTOR('',#11597,1.);
#3136=VECTOR('',#11598,1.);
#3137=VECTOR('',#11599,1.);
#3138=VECTOR('',#11602,1.);
#3139=VECTOR('',#11603,1.);
#3140=VECTOR('',#11604,1.);
#3141=VECTOR('',#11607,1.);
#3142=VECTOR('',#11608,1.);
#3143=VECTOR('',#11609,1.);
#3144=VECTOR('',#11612,1.);
#3145=VECTOR('',#11613,1.);
#3146=VECTOR('',#11622,1.);
#3147=VECTOR('',#11623,1.);
#3148=VECTOR('',#11624,1.);
#3149=VECTOR('',#11625,1.);
#3150=VECTOR('',#11628,1.);
#3151=VECTOR('',#11629,1.);
#3152=VECTOR('',#11630,1.);
#3153=VECTOR('',#11633,1.);
#3154=VECTOR('',#11634,1.);
#3155=VECTOR('',#11635,1.);
#3156=VECTOR('',#11638,1.);
#3157=VECTOR('',#11639,1.);
#3158=VECTOR('',#11640,1.);
#3159=VECTOR('',#11643,1.);
#3160=VECTOR('',#11644,1.);
#3161=VECTOR('',#11645,1.);
#3162=VECTOR('',#11648,1.);
#3163=VECTOR('',#11649,1.);
#3164=VECTOR('',#11650,1.);
#3165=VECTOR('',#11653,1.);
#3166=VECTOR('',#11654,1.);
#3167=VECTOR('',#11655,1.);
#3168=VECTOR('',#11658,1.);
#3169=VECTOR('',#11659,1.);
#3170=VECTOR('',#11674,1.);
#3171=VECTOR('',#11675,1.);
#3172=VECTOR('',#11676,1.);
#3173=VECTOR('',#11677,1.);
#3174=VECTOR('',#11680,1.);
#3175=VECTOR('',#11681,1.);
#3176=VECTOR('',#11682,1.);
#3177=VECTOR('',#11685,1.);
#3178=VECTOR('',#11686,1.);
#3179=VECTOR('',#11687,1.);
#3180=VECTOR('',#11690,1.);
#3181=VECTOR('',#11691,1.);
#3182=VECTOR('',#11692,1.);
#3183=VECTOR('',#11695,1.);
#3184=VECTOR('',#11696,1.);
#3185=VECTOR('',#11697,1.);
#3186=VECTOR('',#11700,1.);
#3187=VECTOR('',#11701,1.);
#3188=VECTOR('',#11718,0.4);
#3189=VECTOR('',#11723,0.425);
#3190=VECTOR('',#11728,0.41);
#3191=VECTOR('',#11737,0.26);
#3192=VECTOR('',#11740,0.25);
#3193=VECTOR('',#11745,1.);
#3194=VECTOR('',#11746,1.);
#3195=VECTOR('',#11747,1.);
#3196=VECTOR('',#11748,1.);
#3197=VECTOR('',#11751,1.);
#3198=VECTOR('',#11752,1.);
#3199=VECTOR('',#11753,1.);
#3200=VECTOR('',#11756,1.);
#3201=VECTOR('',#11757,1.);
#3202=VECTOR('',#11758,1.);
#3203=VECTOR('',#11761,1.);
#3204=VECTOR('',#11762,1.);
#3205=VECTOR('',#11763,1.);
#3206=VECTOR('',#11766,1.);
#3207=VECTOR('',#11767,1.);
#3208=VECTOR('',#11768,1.);
#3209=VECTOR('',#11771,1.);
#3210=VECTOR('',#11772,1.);
#3211=VECTOR('',#11789,0.325);
#3212=VECTOR('',#11794,0.35);
#3213=VECTOR('',#11799,0.335);
#3214=VECTOR('',#11808,0.21);
#3215=VECTOR('',#11811,0.2);
#3216=CIRCLE('',#8388,0.21);
#3217=CIRCLE('',#8389,0.21);
#3218=CIRCLE('',#8391,0.21);
#3219=CIRCLE('',#8392,0.21);
#3220=CIRCLE('',#8394,0.21);
#3221=CIRCLE('',#8395,0.21);
#3222=CIRCLE('',#8397,0.21);
#3223=CIRCLE('',#8398,0.21);
#3224=CIRCLE('',#8400,0.21);
#3225=CIRCLE('',#8401,0.21);
#3226=CIRCLE('',#8403,0.21);
#3227=CIRCLE('',#8404,0.21);
#3228=CIRCLE('',#8406,0.21);
#3229=CIRCLE('',#8407,0.21);
#3230=CIRCLE('',#8409,0.21);
#3231=CIRCLE('',#8410,0.21);
#3232=CIRCLE('',#8412,0.164999999999999);
#3233=CIRCLE('',#8413,0.164999999999999);
#3234=CIRCLE('',#8415,0.164999999999999);
#3235=CIRCLE('',#8416,0.164999999999999);
#3236=CIRCLE('',#8418,0.165);
#3237=CIRCLE('',#8419,0.165);
#3238=CIRCLE('',#8421,0.165);
#3239=CIRCLE('',#8422,0.165);
#3240=CIRCLE('',#8446,0.165);
#3241=CIRCLE('',#8447,0.165);
#3242=CIRCLE('',#8450,0.165);
#3243=CIRCLE('',#8451,0.165);
#3244=CIRCLE('',#8454,0.165);
#3245=CIRCLE('',#8455,0.165);
#3246=CIRCLE('',#8458,0.165);
#3247=CIRCLE('',#8459,0.165);
#3248=CIRCLE('',#8462,0.525);
#3249=CIRCLE('',#8463,0.525);
#3250=CIRCLE('',#8465,2.2);
#3251=CIRCLE('',#8467,0.525);
#3252=CIRCLE('',#8468,0.525);
#3253=CIRCLE('',#8470,2.2);
#3254=CIRCLE('',#8472,0.525);
#3255=CIRCLE('',#8473,0.525);
#3256=CIRCLE('',#8475,2.2);
#3257=CIRCLE('',#8477,0.525);
#3258=CIRCLE('',#8478,0.525);
#3259=CIRCLE('',#8480,2.2);
#3260=CIRCLE('',#8482,2.9);
#3261=CIRCLE('',#8483,2.2);
#3262=CIRCLE('',#8484,2.2);
#3263=CIRCLE('',#8485,2.2);
#3264=CIRCLE('',#8486,2.2);
#3265=CIRCLE('',#8487,2.2);
#3266=CIRCLE('',#8488,0.275);
#3267=CIRCLE('',#8489,0.275);
#3268=CIRCLE('',#8490,0.275);
#3269=CIRCLE('',#8491,0.275);
#3270=CIRCLE('',#8493,0.275);
#3271=CIRCLE('',#8495,0.275);
#3272=CIRCLE('',#8497,0.275);
#3273=CIRCLE('',#8499,0.275);
#3274=CIRCLE('',#8501,2.2);
#3275=CIRCLE('',#8503,1.5);
#3276=CIRCLE('',#8504,1.5);
#3277=CIRCLE('',#8506,1.02);
#3278=CIRCLE('',#8508,2.9);
#3279=CIRCLE('',#8510,1.02);
#3280=CIRCLE('',#8515,0.375);
#3281=CIRCLE('',#8516,0.375);
#3282=CIRCLE('',#8518,0.225);
#3283=CIRCLE('',#8520,0.375);
#3284=CIRCLE('',#8521,0.375);
#3285=CIRCLE('',#8523,0.225);
#3286=CIRCLE('',#8525,0.375);
#3287=CIRCLE('',#8526,0.375);
#3288=CIRCLE('',#8528,0.225);
#3289=CIRCLE('',#8530,0.375);
#3290=CIRCLE('',#8531,0.375);
#3291=CIRCLE('',#8533,0.225);
#3292=CIRCLE('',#8535,0.225);
#3293=CIRCLE('',#8537,0.225);
#3294=CIRCLE('',#8539,0.225);
#3295=CIRCLE('',#8541,0.225);
#3296=CIRCLE('',#8543,1.49);
#3297=CIRCLE('',#8544,1.49);
#3298=CIRCLE('',#8546,0.71);
#3299=CIRCLE('',#8548,0.71);
#3300=CIRCLE('',#8550,2.2);
#3301=CIRCLE('',#8551,2.2);
#3302=CIRCLE('',#8557,0.165);
#3303=CIRCLE('',#8558,0.165);
#3304=CIRCLE('',#8561,0.165);
#3305=CIRCLE('',#8562,0.165);
#3306=CIRCLE('',#8565,0.165);
#3307=CIRCLE('',#8566,0.165);
#3308=CIRCLE('',#8569,0.165);
#3309=CIRCLE('',#8570,0.165);
#3310=CIRCLE('',#8573,0.525);
#3311=CIRCLE('',#8574,0.525);
#3312=CIRCLE('',#8576,2.2);
#3313=CIRCLE('',#8578,0.525);
#3314=CIRCLE('',#8579,0.525);
#3315=CIRCLE('',#8581,2.2);
#3316=CIRCLE('',#8583,0.525);
#3317=CIRCLE('',#8584,0.525);
#3318=CIRCLE('',#8586,2.2);
#3319=CIRCLE('',#8588,0.525);
#3320=CIRCLE('',#8589,0.525);
#3321=CIRCLE('',#8591,2.2);
#3322=CIRCLE('',#8593,2.9);
#3323=CIRCLE('',#8594,2.2);
#3324=CIRCLE('',#8595,2.2);
#3325=CIRCLE('',#8596,2.2);
#3326=CIRCLE('',#8597,2.2);
#3327=CIRCLE('',#8598,2.2);
#3328=CIRCLE('',#8599,0.275);
#3329=CIRCLE('',#8600,0.275);
#3330=CIRCLE('',#8601,0.275);
#3331=CIRCLE('',#8602,0.275);
#3332=CIRCLE('',#8604,0.275);
#3333=CIRCLE('',#8606,0.275);
#3334=CIRCLE('',#8608,0.275);
#3335=CIRCLE('',#8610,0.275);
#3336=CIRCLE('',#8612,2.2);
#3337=CIRCLE('',#8614,1.5);
#3338=CIRCLE('',#8615,1.5);
#3339=CIRCLE('',#8617,1.02);
#3340=CIRCLE('',#8619,2.9);
#3341=CIRCLE('',#8621,1.02);
#3342=CIRCLE('',#8626,0.375);
#3343=CIRCLE('',#8627,0.375);
#3344=CIRCLE('',#8629,0.225);
#3345=CIRCLE('',#8631,0.375);
#3346=CIRCLE('',#8632,0.375);
#3347=CIRCLE('',#8634,0.225);
#3348=CIRCLE('',#8636,0.375);
#3349=CIRCLE('',#8637,0.375);
#3350=CIRCLE('',#8639,0.225);
#3351=CIRCLE('',#8641,0.375);
#3352=CIRCLE('',#8642,0.375);
#3353=CIRCLE('',#8644,0.225);
#3354=CIRCLE('',#8646,0.225);
#3355=CIRCLE('',#8648,0.225);
#3356=CIRCLE('',#8650,0.225);
#3357=CIRCLE('',#8652,0.225);
#3358=CIRCLE('',#8654,1.49);
#3359=CIRCLE('',#8655,1.49);
#3360=CIRCLE('',#8657,0.71);
#3361=CIRCLE('',#8659,0.71);
#3362=CIRCLE('',#8661,2.2);
#3363=CIRCLE('',#8662,2.2);
#3364=CIRCLE('',#8667,0.375);
#3365=CIRCLE('',#8668,0.375);
#3366=CIRCLE('',#8670,0.225);
#3367=CIRCLE('',#8672,0.375);
#3368=CIRCLE('',#8673,0.375);
#3369=CIRCLE('',#8675,0.225);
#3370=CIRCLE('',#8677,0.375);
#3371=CIRCLE('',#8678,0.375);
#3372=CIRCLE('',#8680,0.225);
#3373=CIRCLE('',#8682,0.375);
#3374=CIRCLE('',#8683,0.375);
#3375=CIRCLE('',#8685,0.225000000000001);
#3376=CIRCLE('',#8687,0.225);
#3377=CIRCLE('',#8689,0.225);
#3378=CIRCLE('',#8691,0.225);
#3379=CIRCLE('',#8693,0.225000000000001);
#3380=CIRCLE('',#8711,0.976185);
#3381=CIRCLE('',#8712,0.976185);
#3382=CIRCLE('',#8713,0.247676);
#3383=CIRCLE('',#8714,0.976185);
#3384=CIRCLE('',#8715,0.976185);
#3385=CIRCLE('',#8717,0.976185);
#3386=CIRCLE('',#8719,0.5);
#3387=CIRCLE('',#8720,0.5);
#3388=CIRCLE('',#8722,0.56);
#3389=CIRCLE('',#8725,0.976185);
#3390=CIRCLE('',#8727,0.56);
#3391=CIRCLE('',#8731,1.023815);
#3392=CIRCLE('',#8732,1.023815);
#3393=CIRCLE('',#8733,0.247676);
#3394=CIRCLE('',#8734,1.023815);
#3395=CIRCLE('',#8735,1.023815);
#3396=CIRCLE('',#8737,1.023815);
#3397=CIRCLE('',#8739,1.44);
#3398=CIRCLE('',#8740,1.023815);
#3399=CIRCLE('',#8742,1.5);
#3400=CIRCLE('',#8744,1.5);
#3401=CIRCLE('',#8746,1.44);
#3402=CIRCLE('',#8751,0.23815);
#3403=CIRCLE('',#8753,0.23815);
#3404=CIRCLE('',#8755,0.23815);
#3405=CIRCLE('',#8757,0.23815);
#3406=CIRCLE('',#8759,0.23815);
#3407=CIRCLE('',#8761,0.23815);
#3408=CIRCLE('',#8763,0.23815);
#3409=CIRCLE('',#8765,0.23815);
#3410=CIRCLE('',#8768,0.243053047864041);
#3411=CIRCLE('',#8769,0.243053047864041);
#3412=CIRCLE('',#8771,1.019052);
#3413=CIRCLE('',#8772,1.019052);
#3414=CIRCLE('',#8773,1.019052);
#3415=CIRCLE('',#8774,1.019052);
#3416=CIRCLE('',#8775,1.019052);
#3417=CIRCLE('',#8776,1.019052);
#3418=CIRCLE('',#8777,1.019052);
#3419=CIRCLE('',#8778,1.019052);
#3420=CIRCLE('',#8779,1.019052);
#3421=CIRCLE('',#8781,0.980948);
#3422=CIRCLE('',#8782,0.243053047864041);
#3423=CIRCLE('',#8784,0.243053047864041);
#3424=CIRCLE('',#8786,0.980948);
#3425=CIRCLE('',#8787,0.243053047864041);
#3426=CIRCLE('',#8789,0.243053047864041);
#3427=CIRCLE('',#8791,0.980948);
#3428=CIRCLE('',#8792,0.243053047864041);
#3429=CIRCLE('',#8794,0.243053047864041);
#3430=CIRCLE('',#8796,0.980948);
#3431=CIRCLE('',#8797,0.243053047864041);
#3432=CIRCLE('',#8799,0.243053047864041);
#3433=CIRCLE('',#8801,0.980948);
#3434=CIRCLE('',#8802,0.243053047864041);
#3435=CIRCLE('',#8804,0.243053047864041);
#3436=CIRCLE('',#8806,0.980948);
#3437=CIRCLE('',#8807,0.243053047864041);
#3438=CIRCLE('',#8809,0.243053047864041);
#3439=CIRCLE('',#8811,0.980948);
#3440=CIRCLE('',#8812,0.980948);
#3441=CIRCLE('',#8813,0.980948);
#3442=CIRCLE('',#8815,0.243053047864041);
#3443=CIRCLE('',#8817,0.243053047864041);
#3444=CIRCLE('',#8822,1.013815);
#3445=CIRCLE('',#8823,0.991185);
#3446=CIRCLE('',#8825,1.013815);
#3447=CIRCLE('',#8827,0.991185);
#3448=CIRCLE('',#8830,1.013815);
#3449=CIRCLE('',#8831,0.991185);
#3450=CIRCLE('',#8833,1.013815);
#3451=CIRCLE('',#8835,0.991185);
#3452=CIRCLE('',#8845,0.225);
#3453=CIRCLE('',#8846,0.225);
#3454=CIRCLE('',#8848,0.7);
#3455=CIRCLE('',#8849,0.7);
#3456=CIRCLE('',#8852,1.2);
#3457=CIRCLE('',#8853,0.7);
#3458=CIRCLE('',#8854,1.2);
#3459=CIRCLE('',#8855,0.25);
#3460=CIRCLE('',#8856,0.7);
#3461=CIRCLE('',#8859,1.2);
#3462=CIRCLE('',#8861,0.25);
#3463=CIRCLE('',#8863,0.7);
#3464=CIRCLE('',#8866,1.2);
#3465=CIRCLE('',#8870,0.7);
#3466=CIRCLE('',#8871,0.5);
#3467=CIRCLE('',#8874,0.5);
#3468=CIRCLE('',#8878,0.165);
#3469=CIRCLE('',#8879,0.165);
#3470=CIRCLE('',#8882,0.6);
#3471=CIRCLE('',#8883,0.6);
#3472=CIRCLE('',#8888,0.505);
#3473=CIRCLE('',#8889,0.505);
#3474=CIRCLE('',#8891,0.7);
#3475=CIRCLE('',#8892,0.7);
#3476=CIRCLE('',#8897,0.165);
#3477=CIRCLE('',#8899,0.165);
#3478=CIRCLE('',#8902,0.505);
#3479=CIRCLE('',#8903,0.505);
#3480=CIRCLE('',#8905,0.9);
#3481=CIRCLE('',#8906,0.9);
#3482=CIRCLE('',#8911,0.165);
#3483=CIRCLE('',#8912,0.165);
#3484=CIRCLE('',#8915,0.7);
#3485=CIRCLE('',#8916,0.3);
#3486=CIRCLE('',#8918,0.7);
#3487=CIRCLE('',#8919,0.3);
#3488=CIRCLE('',#8922,0.3);
#3489=CIRCLE('',#8924,0.3);
#3490=CIRCLE('',#8929,0.305);
#3491=CIRCLE('',#8930,0.305);
#3492=CIRCLE('',#8932,0.5);
#3493=CIRCLE('',#8933,0.5);
#3494=CIRCLE('',#8938,0.305);
#3495=CIRCLE('',#8939,0.305);
#3496=CIRCLE('',#8941,0.5);
#3497=CIRCLE('',#8942,0.5);
#3498=CIRCLE('',#8947,0.225);
#3499=CIRCLE('',#8948,0.225);
#3500=CIRCLE('',#8950,0.5);
#3501=CIRCLE('',#8951,0.5);
#3502=CIRCLE('',#8956,0.3);
#3503=CIRCLE('',#8958,0.35);
#3504=CIRCLE('',#8960,0.35);
#3505=CIRCLE('',#8962,0.32);
#3506=CIRCLE('',#8964,0.22);
#3507=CIRCLE('',#8966,0.1954);
#3508=CIRCLE('',#8968,0.1954);
#3509=CIRCLE('',#8970,0.16);
#3510=CIRCLE('',#8983,0.25);
#3511=CIRCLE('',#8984,0.25);
#3512=CIRCLE('',#8990,1.2);
#3513=CIRCLE('',#8991,1.2);
#3514=CIRCLE('',#8993,1.2);
#3515=CIRCLE('',#8994,0.7);
#3516=CIRCLE('',#8998,1.2);
#3517=CIRCLE('',#9000,0.7);
#3518=CIRCLE('',#9001,0.5);
#3519=CIRCLE('',#9004,0.5);
#3520=CIRCLE('',#9009,0.505);
#3521=CIRCLE('',#9010,0.505);
#3522=CIRCLE('',#9012,0.7);
#3523=CIRCLE('',#9013,0.7);
#3524=CIRCLE('',#9018,0.165);
#3525=CIRCLE('',#9020,0.165);
#3526=CIRCLE('',#9023,0.505);
#3527=CIRCLE('',#9024,0.505);
#3528=CIRCLE('',#9026,0.9);
#3529=CIRCLE('',#9027,0.9);
#3530=CIRCLE('',#9032,0.165);
#3531=CIRCLE('',#9033,0.165);
#3532=CIRCLE('',#9036,0.7);
#3533=CIRCLE('',#9037,0.3);
#3534=CIRCLE('',#9039,0.7);
#3535=CIRCLE('',#9040,0.3);
#3536=CIRCLE('',#9043,0.3);
#3537=CIRCLE('',#9045,0.3);
#3538=CIRCLE('',#9050,0.305);
#3539=CIRCLE('',#9051,0.305);
#3540=CIRCLE('',#9053,0.5);
#3541=CIRCLE('',#9054,0.5);
#3542=CIRCLE('',#9059,0.305);
#3543=CIRCLE('',#9060,0.305);
#3544=CIRCLE('',#9062,0.5);
#3545=CIRCLE('',#9063,0.5);
#3546=CIRCLE('',#9068,0.225);
#3547=CIRCLE('',#9069,0.225);
#3548=CIRCLE('',#9071,0.5);
#3549=CIRCLE('',#9072,0.5);
#3550=CIRCLE('',#9077,0.1954);
#3551=CIRCLE('',#9086,0.17);
#3552=CIRCLE('',#9088,0.1954);
#3553=CIRCLE('',#9093,0.305);
#3554=CIRCLE('',#9094,0.305);
#3555=CIRCLE('',#9113,0.5);
#3556=CIRCLE('',#9114,0.5);
#3557=CIRCLE('',#9116,0.5);
#3558=CIRCLE('',#9117,0.5);
#3559=CIRCLE('',#9119,0.800000000000001);
#3560=CIRCLE('',#9120,0.800000000000001);
#3561=CIRCLE('',#9123,0.8);
#3562=CIRCLE('',#9126,0.8);
#3563=CIRCLE('',#9130,0.305);
#3564=CIRCLE('',#9131,0.305);
#3565=CIRCLE('',#9133,0.5);
#3566=CIRCLE('',#9134,0.5);
#3567=CIRCLE('',#9139,0.305);
#3568=CIRCLE('',#9140,0.305);
#3569=CIRCLE('',#9142,0.5);
#3570=CIRCLE('',#9143,0.5);
#3571=CIRCLE('',#9152,0.25);
#3572=CIRCLE('',#9153,0.25);
#3573=CIRCLE('',#9155,0.275);
#3574=CIRCLE('',#9156,0.275);
#3575=CIRCLE('',#9158,0.275);
#3576=CIRCLE('',#9159,0.275);
#3577=CIRCLE('',#9161,0.275);
#3578=CIRCLE('',#9162,0.275);
#3579=CIRCLE('',#9164,0.275);
#3580=CIRCLE('',#9165,0.275);
#3581=CIRCLE('',#9174,0.164999999999999);
#3582=CIRCLE('',#9175,0.164999999999999);
#3583=CIRCLE('',#9178,0.699999999999999);
#3584=CIRCLE('',#9179,0.300000000000001);
#3585=CIRCLE('',#9181,0.699999999999999);
#3586=CIRCLE('',#9182,0.300000000000001);
#3587=CIRCLE('',#9185,0.300000000000001);
#3588=CIRCLE('',#9187,0.300000000000001);
#3589=CIRCLE('',#9192,0.305);
#3590=CIRCLE('',#9193,0.305);
#3591=CIRCLE('',#9195,0.5);
#3592=CIRCLE('',#9196,0.5);
#3593=CIRCLE('',#9201,0.305);
#3594=CIRCLE('',#9202,0.305);
#3595=CIRCLE('',#9204,0.5);
#3596=CIRCLE('',#9205,0.5);
#3597=CIRCLE('',#9210,0.225);
#3598=CIRCLE('',#9211,0.225);
#3599=CIRCLE('',#9213,0.5);
#3600=CIRCLE('',#9214,0.5);
#3601=CIRCLE('',#9220,0.21);
#3602=CIRCLE('',#9222,0.21);
#3603=CIRCLE('',#9223,0.21);
#3604=CIRCLE('',#9224,0.21);
#3605=CIRCLE('',#9226,0.21);
#3606=CIRCLE('',#9228,0.21);
#3607=CIRCLE('',#9229,0.21);
#3608=CIRCLE('',#9230,0.21);
#3609=CIRCLE('',#9232,0.21);
#3610=CIRCLE('',#9234,0.21);
#3611=CIRCLE('',#9235,0.21);
#3612=CIRCLE('',#9236,0.21);
#3613=CIRCLE('',#9238,0.21);
#3614=CIRCLE('',#9240,0.21);
#3615=CIRCLE('',#9241,0.21);
#3616=CIRCLE('',#9242,0.21);
#3617=CIRCLE('',#9292,0.24505);
#3618=CIRCLE('',#9294,0.375);
#3619=CIRCLE('',#9296,0.425);
#3620=CIRCLE('',#9298,0.425);
#3621=CIRCLE('',#9300,0.395);
#3622=CIRCLE('',#9302,0.27);
#3623=CIRCLE('',#9304,0.24505);
#3624=CIRCLE('',#9316,0.1954);
#3625=CIRCLE('',#9318,0.3);
#3626=CIRCLE('',#9320,0.35);
#3627=CIRCLE('',#9322,0.35);
#3628=CIRCLE('',#9324,0.32);
#3629=CIRCLE('',#9326,0.22);
#3630=CIRCLE('',#9328,0.1954);
#3631=VERTEX_POINT('',#11950);
#3632=VERTEX_POINT('',#11952);
#3633=VERTEX_POINT('',#11956);
#3634=VERTEX_POINT('',#11958);
#3635=VERTEX_POINT('',#11962);
#3636=VERTEX_POINT('',#11964);
#3637=VERTEX_POINT('',#11968);
#3638=VERTEX_POINT('',#11970);
#3639=VERTEX_POINT('',#11974);
#3640=VERTEX_POINT('',#11976);
#3641=VERTEX_POINT('',#11980);
#3642=VERTEX_POINT('',#11982);
#3643=VERTEX_POINT('',#11986);
#3644=VERTEX_POINT('',#11988);
#3645=VERTEX_POINT('',#11992);
#3646=VERTEX_POINT('',#11994);
#3647=VERTEX_POINT('',#11998);
#3648=VERTEX_POINT('',#12000);
#3649=VERTEX_POINT('',#12004);
#3650=VERTEX_POINT('',#12006);
#3651=VERTEX_POINT('',#12010);
#3652=VERTEX_POINT('',#12012);
#3653=VERTEX_POINT('',#12016);
#3654=VERTEX_POINT('',#12018);
#3655=VERTEX_POINT('',#12022);
#3656=VERTEX_POINT('',#12023);
#3657=VERTEX_POINT('',#12025);
#3658=VERTEX_POINT('',#12027);
#3659=VERTEX_POINT('',#12031);
#3660=VERTEX_POINT('',#12033);
#3661=VERTEX_POINT('',#12037);
#3662=VERTEX_POINT('',#12039);
#3663=VERTEX_POINT('',#12049);
#3664=VERTEX_POINT('',#12050);
#3665=VERTEX_POINT('',#12052);
#3666=VERTEX_POINT('',#12054);
#3667=VERTEX_POINT('',#12058);
#3668=VERTEX_POINT('',#12060);
#3669=VERTEX_POINT('',#12064);
#3670=VERTEX_POINT('',#12066);
#3671=VERTEX_POINT('',#12076);
#3672=VERTEX_POINT('',#12077);
#3673=VERTEX_POINT('',#12079);
#3674=VERTEX_POINT('',#12081);
#3675=VERTEX_POINT('',#12085);
#3676=VERTEX_POINT('',#12087);
#3677=VERTEX_POINT('',#12091);
#3678=VERTEX_POINT('',#12093);
#3679=VERTEX_POINT('',#12103);
#3680=VERTEX_POINT('',#12104);
#3681=VERTEX_POINT('',#12141);
#3682=VERTEX_POINT('',#12143);
#3683=VERTEX_POINT('',#12181);
#3684=VERTEX_POINT('',#12183);
#3685=VERTEX_POINT('',#12188);
#3686=VERTEX_POINT('',#12190);
#3687=VERTEX_POINT('',#12195);
#3688=VERTEX_POINT('',#12197);
#3689=VERTEX_POINT('',#12202);
#3690=VERTEX_POINT('',#12204);
#3691=VERTEX_POINT('',#12209);
#3692=VERTEX_POINT('',#12210);
#3693=VERTEX_POINT('',#12212);
#3694=VERTEX_POINT('',#12214);
#3695=VERTEX_POINT('',#12220);
#3696=VERTEX_POINT('',#12221);
#3697=VERTEX_POINT('',#12223);
#3698=VERTEX_POINT('',#12225);
#3699=VERTEX_POINT('',#12231);
#3700=VERTEX_POINT('',#12232);
#3701=VERTEX_POINT('',#12234);
#3702=VERTEX_POINT('',#12236);
#3703=VERTEX_POINT('',#12242);
#3704=VERTEX_POINT('',#12243);
#3705=VERTEX_POINT('',#12245);
#3706=VERTEX_POINT('',#12247);
#3707=VERTEX_POINT('',#12253);
#3708=VERTEX_POINT('',#12255);
#3709=VERTEX_POINT('',#12261);
#3710=VERTEX_POINT('',#12263);
#3711=VERTEX_POINT('',#12265);
#3712=VERTEX_POINT('',#12267);
#3713=VERTEX_POINT('',#12270);
#3714=VERTEX_POINT('',#12274);
#3715=VERTEX_POINT('',#12278);
#3716=VERTEX_POINT('',#12282);
#3717=VERTEX_POINT('',#12286);
#3718=VERTEX_POINT('',#12290);
#3719=VERTEX_POINT('',#12292);
#3720=VERTEX_POINT('',#12296);
#3721=VERTEX_POINT('',#12299);
#3722=VERTEX_POINT('',#12303);
#3723=VERTEX_POINT('',#12310);
#3724=VERTEX_POINT('',#12312);
#3725=VERTEX_POINT('',#12316);
#3726=VERTEX_POINT('',#12319);
#3727=VERTEX_POINT('',#12321);
#3728=VERTEX_POINT('',#12325);
#3729=VERTEX_POINT('',#12328);
#3730=VERTEX_POINT('',#12330);
#3731=VERTEX_POINT('',#12334);
#3732=VERTEX_POINT('',#12337);
#3733=VERTEX_POINT('',#12339);
#3734=VERTEX_POINT('',#12343);
#3735=VERTEX_POINT('',#12346);
#3736=VERTEX_POINT('',#12350);
#3737=VERTEX_POINT('',#12354);
#3738=VERTEX_POINT('',#12358);
#3739=VERTEX_POINT('',#12362);
#3740=VERTEX_POINT('',#12364);
#3741=VERTEX_POINT('',#12368);
#3742=VERTEX_POINT('',#12371);
#3743=VERTEX_POINT('',#12375);
#3744=VERTEX_POINT('',#12377);
#3745=VERTEX_POINT('',#12384);
#3746=VERTEX_POINT('',#12385);
#3747=VERTEX_POINT('',#12422);
#3748=VERTEX_POINT('',#12424);
#3749=VERTEX_POINT('',#12462);
#3750=VERTEX_POINT('',#12464);
#3751=VERTEX_POINT('',#12469);
#3752=VERTEX_POINT('',#12471);
#3753=VERTEX_POINT('',#12476);
#3754=VERTEX_POINT('',#12478);
#3755=VERTEX_POINT('',#12483);
#3756=VERTEX_POINT('',#12485);
#3757=VERTEX_POINT('',#12490);
#3758=VERTEX_POINT('',#12491);
#3759=VERTEX_POINT('',#12493);
#3760=VERTEX_POINT('',#12495);
#3761=VERTEX_POINT('',#12501);
#3762=VERTEX_POINT('',#12502);
#3763=VERTEX_POINT('',#12504);
#3764=VERTEX_POINT('',#12506);
#3765=VERTEX_POINT('',#12512);
#3766=VERTEX_POINT('',#12513);
#3767=VERTEX_POINT('',#12515);
#3768=VERTEX_POINT('',#12517);
#3769=VERTEX_POINT('',#12523);
#3770=VERTEX_POINT('',#12524);
#3771=VERTEX_POINT('',#12526);
#3772=VERTEX_POINT('',#12528);
#3773=VERTEX_POINT('',#12534);
#3774=VERTEX_POINT('',#12536);
#3775=VERTEX_POINT('',#12542);
#3776=VERTEX_POINT('',#12544);
#3777=VERTEX_POINT('',#12546);
#3778=VERTEX_POINT('',#12548);
#3779=VERTEX_POINT('',#12551);
#3780=VERTEX_POINT('',#12555);
#3781=VERTEX_POINT('',#12559);
#3782=VERTEX_POINT('',#12563);
#3783=VERTEX_POINT('',#12567);
#3784=VERTEX_POINT('',#12571);
#3785=VERTEX_POINT('',#12573);
#3786=VERTEX_POINT('',#12577);
#3787=VERTEX_POINT('',#12580);
#3788=VERTEX_POINT('',#12584);
#3789=VERTEX_POINT('',#12591);
#3790=VERTEX_POINT('',#12593);
#3791=VERTEX_POINT('',#12597);
#3792=VERTEX_POINT('',#12600);
#3793=VERTEX_POINT('',#12602);
#3794=VERTEX_POINT('',#12606);
#3795=VERTEX_POINT('',#12609);
#3796=VERTEX_POINT('',#12611);
#3797=VERTEX_POINT('',#12615);
#3798=VERTEX_POINT('',#12618);
#3799=VERTEX_POINT('',#12620);
#3800=VERTEX_POINT('',#12624);
#3801=VERTEX_POINT('',#12627);
#3802=VERTEX_POINT('',#12631);
#3803=VERTEX_POINT('',#12635);
#3804=VERTEX_POINT('',#12639);
#3805=VERTEX_POINT('',#12643);
#3806=VERTEX_POINT('',#12645);
#3807=VERTEX_POINT('',#12649);
#3808=VERTEX_POINT('',#12652);
#3809=VERTEX_POINT('',#12656);
#3810=VERTEX_POINT('',#12658);
#3811=VERTEX_POINT('',#12665);
#3812=VERTEX_POINT('',#12667);
#3813=VERTEX_POINT('',#12671);
#3814=VERTEX_POINT('',#12674);
#3815=VERTEX_POINT('',#12676);
#3816=VERTEX_POINT('',#12680);
#3817=VERTEX_POINT('',#12683);
#3818=VERTEX_POINT('',#12685);
#3819=VERTEX_POINT('',#12689);
#3820=VERTEX_POINT('',#12692);
#3821=VERTEX_POINT('',#12694);
#3822=VERTEX_POINT('',#12698);
#3823=VERTEX_POINT('',#12701);
#3824=VERTEX_POINT('',#12705);
#3825=VERTEX_POINT('',#12709);
#3826=VERTEX_POINT('',#12713);
#3827=VERTEX_POINT('',#12717);
#3828=VERTEX_POINT('',#12718);
#3829=VERTEX_POINT('',#12720);
#3830=VERTEX_POINT('',#12722);
#3831=VERTEX_POINT('',#12726);
#3832=VERTEX_POINT('',#12728);
#3833=VERTEX_POINT('',#12732);
#3834=VERTEX_POINT('',#12734);
#3835=VERTEX_POINT('',#12738);
#3836=VERTEX_POINT('',#12740);
#3837=VERTEX_POINT('',#12744);
#3838=VERTEX_POINT('',#12746);
#3839=VERTEX_POINT('',#12750);
#3840=VERTEX_POINT('',#12752);
#3841=VERTEX_POINT('',#12756);
#3842=VERTEX_POINT('',#12758);
#3843=VERTEX_POINT('',#12762);
#3844=VERTEX_POINT('',#12764);
#3845=VERTEX_POINT('',#12768);
#3846=VERTEX_POINT('',#12770);
#3847=VERTEX_POINT('',#12774);
#3848=VERTEX_POINT('',#12776);
#3849=VERTEX_POINT('',#12780);
#3850=VERTEX_POINT('',#12782);
#3851=VERTEX_POINT('',#12793);
#3852=VERTEX_POINT('',#12794);
#3853=VERTEX_POINT('',#12797);
#3854=VERTEX_POINT('',#12799);
#3855=VERTEX_POINT('',#12803);
#3856=VERTEX_POINT('',#12807);
#3857=VERTEX_POINT('',#12809);
#3858=VERTEX_POINT('',#12813);
#3859=VERTEX_POINT('',#12818);
#3860=VERTEX_POINT('',#12822);
#3861=VERTEX_POINT('',#12828);
#3862=VERTEX_POINT('',#12829);
#3863=VERTEX_POINT('',#12832);
#3864=VERTEX_POINT('',#12834);
#3865=VERTEX_POINT('',#12838);
#3866=VERTEX_POINT('',#12842);
#3867=VERTEX_POINT('',#12844);
#3868=VERTEX_POINT('',#12847);
#3869=VERTEX_POINT('',#12851);
#3870=VERTEX_POINT('',#12855);
#3871=VERTEX_POINT('',#12863);
#3872=VERTEX_POINT('',#12864);
#3873=VERTEX_POINT('',#12867);
#3874=VERTEX_POINT('',#12868);
#3875=VERTEX_POINT('',#12871);
#3876=VERTEX_POINT('',#12872);
#3877=VERTEX_POINT('',#12875);
#3878=VERTEX_POINT('',#12876);
#3879=VERTEX_POINT('',#12879);
#3880=VERTEX_POINT('',#12880);
#3881=VERTEX_POINT('',#12883);
#3882=VERTEX_POINT('',#12884);
#3883=VERTEX_POINT('',#12887);
#3884=VERTEX_POINT('',#12888);
#3885=VERTEX_POINT('',#12891);
#3886=VERTEX_POINT('',#12892);
#3887=VERTEX_POINT('',#12896);
#3888=VERTEX_POINT('',#12897);
#3889=VERTEX_POINT('',#12920);
#3890=VERTEX_POINT('',#12922);
#3891=VERTEX_POINT('',#12947);
#3892=VERTEX_POINT('',#12949);
#3893=VERTEX_POINT('',#12972);
#3894=VERTEX_POINT('',#12974);
#3895=VERTEX_POINT('',#12997);
#3896=VERTEX_POINT('',#12999);
#3897=VERTEX_POINT('',#13012);
#3898=VERTEX_POINT('',#13015);
#3899=VERTEX_POINT('',#13028);
#3900=VERTEX_POINT('',#13030);
#3901=VERTEX_POINT('',#13053);
#3902=VERTEX_POINT('',#13055);
#3903=VERTEX_POINT('',#13078);
#3904=VERTEX_POINT('',#13080);
#3905=VERTEX_POINT('',#13103);
#3906=VERTEX_POINT('',#13105);
#3907=VERTEX_POINT('',#13130);
#3908=VERTEX_POINT('',#13134);
#3909=VERTEX_POINT('',#13159);
#3910=VERTEX_POINT('',#13163);
#3911=VERTEX_POINT('',#13188);
#3912=VERTEX_POINT('',#13192);
#3913=VERTEX_POINT('',#13193);
#3914=VERTEX_POINT('',#13220);
#3915=VERTEX_POINT('',#13224);
#3916=VERTEX_POINT('',#13249);
#3917=VERTEX_POINT('',#13253);
#3918=VERTEX_POINT('',#13278);
#3919=VERTEX_POINT('',#13282);
#3920=VERTEX_POINT('',#13307);
#3921=VERTEX_POINT('',#13310);
#3922=VERTEX_POINT('',#13312);
#3923=VERTEX_POINT('',#13344);
#3924=VERTEX_POINT('',#13346);
#3925=VERTEX_POINT('',#13349);
#3926=VERTEX_POINT('',#13353);
#3927=VERTEX_POINT('',#13358);
#3928=VERTEX_POINT('',#13360);
#3929=VERTEX_POINT('',#13363);
#3930=VERTEX_POINT('',#13367);
#3931=VERTEX_POINT('',#13379);
#3932=VERTEX_POINT('',#13381);
#3933=VERTEX_POINT('',#13385);
#3934=VERTEX_POINT('',#13386);
#3935=VERTEX_POINT('',#13388);
#3936=VERTEX_POINT('',#13390);
#3937=VERTEX_POINT('',#13394);
#3938=VERTEX_POINT('',#13396);
#3939=VERTEX_POINT('',#13400);
#3940=VERTEX_POINT('',#13402);
#3941=VERTEX_POINT('',#13404);
#3942=VERTEX_POINT('',#13406);
#3943=VERTEX_POINT('',#13408);
#3944=VERTEX_POINT('',#13411);
#3945=VERTEX_POINT('',#13413);
#3946=VERTEX_POINT('',#13416);
#3947=VERTEX_POINT('',#13420);
#3948=VERTEX_POINT('',#13424);
#3949=VERTEX_POINT('',#13428);
#3950=VERTEX_POINT('',#13430);
#3951=VERTEX_POINT('',#13434);
#3952=VERTEX_POINT('',#13443);
#3953=VERTEX_POINT('',#13445);
#3954=VERTEX_POINT('',#13450);
#3955=VERTEX_POINT('',#13456);
#3956=VERTEX_POINT('',#13458);
#3957=VERTEX_POINT('',#13463);
#3958=VERTEX_POINT('',#13465);
#3959=VERTEX_POINT('',#13472);
#3960=VERTEX_POINT('',#13474);
#3961=VERTEX_POINT('',#13478);
#3962=VERTEX_POINT('',#13480);
#3963=VERTEX_POINT('',#13487);
#3964=VERTEX_POINT('',#13488);
#3965=VERTEX_POINT('',#13492);
#3966=VERTEX_POINT('',#13507);
#3967=VERTEX_POINT('',#13509);
#3968=VERTEX_POINT('',#13518);
#3969=VERTEX_POINT('',#13520);
#3970=VERTEX_POINT('',#13568);
#3971=VERTEX_POINT('',#13570);
#3972=VERTEX_POINT('',#13574);
#3973=VERTEX_POINT('',#13576);
#3974=VERTEX_POINT('',#13583);
#3975=VERTEX_POINT('',#13585);
#3976=VERTEX_POINT('',#13590);
#3977=VERTEX_POINT('',#13592);
#3978=VERTEX_POINT('',#13595);
#3979=VERTEX_POINT('',#13597);
#3980=VERTEX_POINT('',#13602);
#3981=VERTEX_POINT('',#13606);
#3982=VERTEX_POINT('',#13613);
#3983=VERTEX_POINT('',#13615);
#3984=VERTEX_POINT('',#13619);
#3985=VERTEX_POINT('',#13621);
#3986=VERTEX_POINT('',#13628);
#3987=VERTEX_POINT('',#13630);
#3988=VERTEX_POINT('',#13634);
#3989=VERTEX_POINT('',#13636);
#3990=VERTEX_POINT('',#13643);
#3991=VERTEX_POINT('',#13645);
#3992=VERTEX_POINT('',#13649);
#3993=VERTEX_POINT('',#13651);
#3994=VERTEX_POINT('',#13658);
#3995=VERTEX_POINT('',#13661);
#3996=VERTEX_POINT('',#13665);
#3997=VERTEX_POINT('',#13669);
#3998=VERTEX_POINT('',#13673);
#3999=VERTEX_POINT('',#13676);
#4000=VERTEX_POINT('',#13680);
#4001=VERTEX_POINT('',#13684);
#4002=VERTEX_POINT('',#13689);
#4003=VERTEX_POINT('',#13690);
#4004=VERTEX_POINT('',#13692);
#4005=VERTEX_POINT('',#13694);
#4006=VERTEX_POINT('',#13698);
#4007=VERTEX_POINT('',#13700);
#4008=VERTEX_POINT('',#13704);
#4009=VERTEX_POINT('',#13706);
#4010=VERTEX_POINT('',#13710);
#4011=VERTEX_POINT('',#13712);
#4012=VERTEX_POINT('',#13716);
#4013=VERTEX_POINT('',#13718);
#4014=VERTEX_POINT('',#13729);
#4015=VERTEX_POINT('',#13731);
#4016=VERTEX_POINT('',#13735);
#4017=VERTEX_POINT('',#13736);
#4018=VERTEX_POINT('',#13738);
#4019=VERTEX_POINT('',#13740);
#4020=VERTEX_POINT('',#13744);
#4021=VERTEX_POINT('',#13746);
#4022=VERTEX_POINT('',#13750);
#4023=VERTEX_POINT('',#13752);
#4024=VERTEX_POINT('',#13759);
#4025=VERTEX_POINT('',#13760);
#4026=VERTEX_POINT('',#13762);
#4027=VERTEX_POINT('',#13764);
#4028=VERTEX_POINT('',#13768);
#4029=VERTEX_POINT('',#13770);
#4030=VERTEX_POINT('',#13773);
#4031=VERTEX_POINT('',#13776);
#4032=VERTEX_POINT('',#13780);
#4033=VERTEX_POINT('',#13786);
#4034=VERTEX_POINT('',#13788);
#4035=VERTEX_POINT('',#13793);
#4036=VERTEX_POINT('',#13800);
#4037=VERTEX_POINT('',#13802);
#4038=VERTEX_POINT('',#13806);
#4039=VERTEX_POINT('',#13808);
#4040=VERTEX_POINT('',#13815);
#4041=VERTEX_POINT('',#13816);
#4042=VERTEX_POINT('',#13820);
#4043=VERTEX_POINT('',#13835);
#4044=VERTEX_POINT('',#13837);
#4045=VERTEX_POINT('',#13846);
#4046=VERTEX_POINT('',#13848);
#4047=VERTEX_POINT('',#13896);
#4048=VERTEX_POINT('',#13898);
#4049=VERTEX_POINT('',#13902);
#4050=VERTEX_POINT('',#13904);
#4051=VERTEX_POINT('',#13911);
#4052=VERTEX_POINT('',#13913);
#4053=VERTEX_POINT('',#13918);
#4054=VERTEX_POINT('',#13920);
#4055=VERTEX_POINT('',#13923);
#4056=VERTEX_POINT('',#13925);
#4057=VERTEX_POINT('',#13930);
#4058=VERTEX_POINT('',#13934);
#4059=VERTEX_POINT('',#13941);
#4060=VERTEX_POINT('',#13943);
#4061=VERTEX_POINT('',#13947);
#4062=VERTEX_POINT('',#13949);
#4063=VERTEX_POINT('',#13956);
#4064=VERTEX_POINT('',#13958);
#4065=VERTEX_POINT('',#13962);
#4066=VERTEX_POINT('',#13964);
#4067=VERTEX_POINT('',#13971);
#4068=VERTEX_POINT('',#13973);
#4069=VERTEX_POINT('',#13977);
#4070=VERTEX_POINT('',#13979);
#4071=VERTEX_POINT('',#13986);
#4072=VERTEX_POINT('',#13989);
#4073=VERTEX_POINT('',#13990);
#4074=VERTEX_POINT('',#13992);
#4075=VERTEX_POINT('',#13994);
#4076=VERTEX_POINT('',#13998);
#4077=VERTEX_POINT('',#14000);
#4078=VERTEX_POINT('',#14004);
#4079=VERTEX_POINT('',#14006);
#4080=VERTEX_POINT('',#14010);
#4081=VERTEX_POINT('',#14012);
#4082=VERTEX_POINT('',#14016);
#4083=VERTEX_POINT('',#14018);
#4084=VERTEX_POINT('',#14026);
#4085=VERTEX_POINT('',#14029);
#4086=VERTEX_POINT('',#14037);
#4087=VERTEX_POINT('',#14039);
#4088=VERTEX_POINT('',#14043);
#4089=VERTEX_POINT('',#14044);
#4090=VERTEX_POINT('',#14046);
#4091=VERTEX_POINT('',#14048);
#4092=VERTEX_POINT('',#14052);
#4093=VERTEX_POINT('',#14053);
#4094=VERTEX_POINT('',#14055);
#4095=VERTEX_POINT('',#14057);
#4096=VERTEX_POINT('',#14061);
#4097=VERTEX_POINT('',#14063);
#4098=VERTEX_POINT('',#14067);
#4099=VERTEX_POINT('',#14069);
#4100=VERTEX_POINT('',#14076);
#4101=VERTEX_POINT('',#14077);
#4102=VERTEX_POINT('',#14079);
#4103=VERTEX_POINT('',#14081);
#4104=VERTEX_POINT('',#14085);
#4105=VERTEX_POINT('',#14086);
#4106=VERTEX_POINT('',#14088);
#4107=VERTEX_POINT('',#14090);
#4108=VERTEX_POINT('',#14094);
#4109=VERTEX_POINT('',#14095);
#4110=VERTEX_POINT('',#14100);
#4111=VERTEX_POINT('',#14101);
#4112=VERTEX_POINT('',#14120);
#4113=VERTEX_POINT('',#14122);
#4114=VERTEX_POINT('',#14126);
#4115=VERTEX_POINT('',#14128);
#4116=VERTEX_POINT('',#14132);
#4117=VERTEX_POINT('',#14133);
#4118=VERTEX_POINT('',#14135);
#4119=VERTEX_POINT('',#14137);
#4120=VERTEX_POINT('',#14141);
#4121=VERTEX_POINT('',#14143);
#4122=VERTEX_POINT('',#14147);
#4123=VERTEX_POINT('',#14151);
#4124=VERTEX_POINT('',#14159);
#4125=VERTEX_POINT('',#14161);
#4126=VERTEX_POINT('',#14165);
#4127=VERTEX_POINT('',#14167);
#4128=VERTEX_POINT('',#14174);
#4129=VERTEX_POINT('',#14176);
#4130=VERTEX_POINT('',#14180);
#4131=VERTEX_POINT('',#14182);
#4132=VERTEX_POINT('',#14193);
#4133=VERTEX_POINT('',#14195);
#4134=VERTEX_POINT('',#14199);
#4135=VERTEX_POINT('',#14201);
#4136=VERTEX_POINT('',#14205);
#4137=VERTEX_POINT('',#14207);
#4138=VERTEX_POINT('',#14211);
#4139=VERTEX_POINT('',#14213);
#4140=VERTEX_POINT('',#14217);
#4141=VERTEX_POINT('',#14219);
#4142=VERTEX_POINT('',#14223);
#4143=VERTEX_POINT('',#14224);
#4144=VERTEX_POINT('',#14226);
#4145=VERTEX_POINT('',#14228);
#4146=VERTEX_POINT('',#14232);
#4147=VERTEX_POINT('',#14234);
#4148=VERTEX_POINT('',#14238);
#4149=VERTEX_POINT('',#14240);
#4150=VERTEX_POINT('',#14250);
#4151=VERTEX_POINT('',#14252);
#4152=VERTEX_POINT('',#14257);
#4153=VERTEX_POINT('',#14259);
#4154=VERTEX_POINT('',#14262);
#4155=VERTEX_POINT('',#14264);
#4156=VERTEX_POINT('',#14269);
#4157=VERTEX_POINT('',#14273);
#4158=VERTEX_POINT('',#14280);
#4159=VERTEX_POINT('',#14282);
#4160=VERTEX_POINT('',#14286);
#4161=VERTEX_POINT('',#14288);
#4162=VERTEX_POINT('',#14295);
#4163=VERTEX_POINT('',#14297);
#4164=VERTEX_POINT('',#14301);
#4165=VERTEX_POINT('',#14303);
#4166=VERTEX_POINT('',#14310);
#4167=VERTEX_POINT('',#14312);
#4168=VERTEX_POINT('',#14316);
#4169=VERTEX_POINT('',#14318);
#4170=VERTEX_POINT('',#14326);
#4171=VERTEX_POINT('',#14327);
#4172=VERTEX_POINT('',#14331);
#4173=VERTEX_POINT('',#14333);
#4174=VERTEX_POINT('',#14335);
#4175=VERTEX_POINT('',#14338);
#4176=VERTEX_POINT('',#14342);
#4177=VERTEX_POINT('',#14343);
#4178=VERTEX_POINT('',#14347);
#4179=VERTEX_POINT('',#14349);
#4180=VERTEX_POINT('',#14351);
#4181=VERTEX_POINT('',#14354);
#4182=VERTEX_POINT('',#14358);
#4183=VERTEX_POINT('',#14359);
#4184=VERTEX_POINT('',#14363);
#4185=VERTEX_POINT('',#14365);
#4186=VERTEX_POINT('',#14367);
#4187=VERTEX_POINT('',#14370);
#4188=VERTEX_POINT('',#14374);
#4189=VERTEX_POINT('',#14375);
#4190=VERTEX_POINT('',#14379);
#4191=VERTEX_POINT('',#14381);
#4192=VERTEX_POINT('',#14383);
#4193=VERTEX_POINT('',#14386);
#4194=VERTEX_POINT('',#14391);
#4195=VERTEX_POINT('',#14393);
#4196=VERTEX_POINT('',#14395);
#4197=VERTEX_POINT('',#14397);
#4198=VERTEX_POINT('',#14402);
#4199=VERTEX_POINT('',#14404);
#4200=VERTEX_POINT('',#14406);
#4201=VERTEX_POINT('',#14408);
#4202=VERTEX_POINT('',#14412);
#4203=VERTEX_POINT('',#14414);
#4204=VERTEX_POINT('',#14416);
#4205=VERTEX_POINT('',#14418);
#4206=VERTEX_POINT('',#14421);
#4207=VERTEX_POINT('',#14423);
#4208=VERTEX_POINT('',#14425);
#4209=VERTEX_POINT('',#14427);
#4210=VERTEX_POINT('',#14431);
#4211=VERTEX_POINT('',#14435);
#4212=VERTEX_POINT('',#14439);
#4213=VERTEX_POINT('',#14443);
#4214=VERTEX_POINT('',#14449);
#4215=VERTEX_POINT('',#14453);
#4216=VERTEX_POINT('',#14457);
#4217=VERTEX_POINT('',#14461);
#4218=VERTEX_POINT('',#14469);
#4219=VERTEX_POINT('',#14470);
#4220=VERTEX_POINT('',#14472);
#4221=VERTEX_POINT('',#14474);
#4222=VERTEX_POINT('',#14478);
#4223=VERTEX_POINT('',#14480);
#4224=VERTEX_POINT('',#14484);
#4225=VERTEX_POINT('',#14486);
#4226=VERTEX_POINT('',#14490);
#4227=VERTEX_POINT('',#14492);
#4228=VERTEX_POINT('',#14496);
#4229=VERTEX_POINT('',#14498);
#4230=VERTEX_POINT('',#14502);
#4231=VERTEX_POINT('',#14504);
#4232=VERTEX_POINT('',#14508);
#4233=VERTEX_POINT('',#14510);
#4234=VERTEX_POINT('',#14520);
#4235=VERTEX_POINT('',#14521);
#4236=VERTEX_POINT('',#14523);
#4237=VERTEX_POINT('',#14525);
#4238=VERTEX_POINT('',#14529);
#4239=VERTEX_POINT('',#14531);
#4240=VERTEX_POINT('',#14535);
#4241=VERTEX_POINT('',#14537);
#4242=VERTEX_POINT('',#14541);
#4243=VERTEX_POINT('',#14543);
#4244=VERTEX_POINT('',#14547);
#4245=VERTEX_POINT('',#14549);
#4246=VERTEX_POINT('',#14553);
#4247=VERTEX_POINT('',#14555);
#4248=VERTEX_POINT('',#14559);
#4249=VERTEX_POINT('',#14561);
#4250=VERTEX_POINT('',#14574);
#4251=VERTEX_POINT('',#14575);
#4252=VERTEX_POINT('',#14577);
#4253=VERTEX_POINT('',#14579);
#4254=VERTEX_POINT('',#14583);
#4255=VERTEX_POINT('',#14585);
#4256=VERTEX_POINT('',#14589);
#4257=VERTEX_POINT('',#14591);
#4258=VERTEX_POINT('',#14595);
#4259=VERTEX_POINT('',#14597);
#4260=VERTEX_POINT('',#14601);
#4261=VERTEX_POINT('',#14603);
#4262=VERTEX_POINT('',#14612);
#4263=VERTEX_POINT('',#14615);
#4264=VERTEX_POINT('',#14618);
#4265=VERTEX_POINT('',#14622);
#4266=VERTEX_POINT('',#14626);
#4267=VERTEX_POINT('',#14630);
#4268=VERTEX_POINT('',#14633);
#4269=VERTEX_POINT('',#14640);
#4270=VERTEX_POINT('',#14641);
#4271=VERTEX_POINT('',#14643);
#4272=VERTEX_POINT('',#14645);
#4273=VERTEX_POINT('',#14649);
#4274=VERTEX_POINT('',#14651);
#4275=VERTEX_POINT('',#14655);
#4276=VERTEX_POINT('',#14657);
#4277=VERTEX_POINT('',#14661);
#4278=VERTEX_POINT('',#14663);
#4279=VERTEX_POINT('',#14667);
#4280=VERTEX_POINT('',#14669);
#4281=VERTEX_POINT('',#14678);
#4282=VERTEX_POINT('',#14681);
#4283=VERTEX_POINT('',#14684);
#4284=VERTEX_POINT('',#14688);
#4285=VERTEX_POINT('',#14692);
#4286=VERTEX_POINT('',#14696);
#4287=VERTEX_POINT('',#14699);
#4288=EDGE_CURVE('',#3631,#3631,#3216,.T.);
#4289=EDGE_CURVE('',#3631,#3632,#2170,.T.);
#4290=EDGE_CURVE('',#3632,#3632,#3217,.T.);
#4291=EDGE_CURVE('',#3633,#3633,#3218,.T.);
#4292=EDGE_CURVE('',#3633,#3634,#2171,.T.);
#4293=EDGE_CURVE('',#3634,#3634,#3219,.T.);
#4294=EDGE_CURVE('',#3635,#3635,#3220,.T.);
#4295=EDGE_CURVE('',#3635,#3636,#2172,.T.);
#4296=EDGE_CURVE('',#3636,#3636,#3221,.T.);
#4297=EDGE_CURVE('',#3637,#3637,#3222,.T.);
#4298=EDGE_CURVE('',#3637,#3638,#2173,.T.);
#4299=EDGE_CURVE('',#3638,#3638,#3223,.T.);
#4300=EDGE_CURVE('',#3639,#3639,#3224,.T.);
#4301=EDGE_CURVE('',#3639,#3640,#2174,.T.);
#4302=EDGE_CURVE('',#3640,#3640,#3225,.T.);
#4303=EDGE_CURVE('',#3641,#3641,#3226,.T.);
#4304=EDGE_CURVE('',#3641,#3642,#2175,.T.);
#4305=EDGE_CURVE('',#3642,#3642,#3227,.T.);
#4306=EDGE_CURVE('',#3643,#3643,#3228,.T.);
#4307=EDGE_CURVE('',#3643,#3644,#2176,.T.);
#4308=EDGE_CURVE('',#3644,#3644,#3229,.T.);
#4309=EDGE_CURVE('',#3645,#3645,#3230,.T.);
#4310=EDGE_CURVE('',#3645,#3646,#2177,.T.);
#4311=EDGE_CURVE('',#3646,#3646,#3231,.T.);
#4312=EDGE_CURVE('',#3647,#3647,#3232,.T.);
#4313=EDGE_CURVE('',#3647,#3648,#2178,.T.);
#4314=EDGE_CURVE('',#3648,#3648,#3233,.T.);
#4315=EDGE_CURVE('',#3649,#3649,#3234,.T.);
#4316=EDGE_CURVE('',#3649,#3650,#2179,.T.);
#4317=EDGE_CURVE('',#3650,#3650,#3235,.T.);
#4318=EDGE_CURVE('',#3651,#3651,#3236,.T.);
#4319=EDGE_CURVE('',#3651,#3652,#2180,.T.);
#4320=EDGE_CURVE('',#3652,#3652,#3237,.T.);
#4321=EDGE_CURVE('',#3653,#3653,#3238,.T.);
#4322=EDGE_CURVE('',#3653,#3654,#2181,.T.);
#4323=EDGE_CURVE('',#3654,#3654,#3239,.T.);
#4324=EDGE_CURVE('',#3655,#3656,#2182,.T.);
#4325=EDGE_CURVE('',#3656,#3657,#2183,.T.);
#4326=EDGE_CURVE('',#3658,#3657,#2184,.T.);
#4327=EDGE_CURVE('',#3655,#3658,#2185,.T.);
#4328=EDGE_CURVE('',#3659,#3655,#2186,.T.);
#4329=EDGE_CURVE('',#3660,#3658,#2187,.T.);
#4330=EDGE_CURVE('',#3659,#3660,#2188,.T.);
#4331=EDGE_CURVE('',#3661,#3659,#2189,.T.);
#4332=EDGE_CURVE('',#3662,#3660,#2190,.T.);
#4333=EDGE_CURVE('',#3661,#3662,#2191,.T.);
#4334=EDGE_CURVE('',#3656,#3661,#2192,.T.);
#4335=EDGE_CURVE('',#3657,#3662,#2193,.T.);
#4336=EDGE_CURVE('',#3663,#3664,#2194,.T.);
#4337=EDGE_CURVE('',#3664,#3665,#2195,.T.);
#4338=EDGE_CURVE('',#3666,#3665,#2196,.T.);
#4339=EDGE_CURVE('',#3663,#3666,#2197,.T.);
#4340=EDGE_CURVE('',#3667,#3663,#2198,.T.);
#4341=EDGE_CURVE('',#3668,#3666,#2199,.T.);
#4342=EDGE_CURVE('',#3667,#3668,#2200,.T.);
#4343=EDGE_CURVE('',#3669,#3667,#2201,.T.);
#4344=EDGE_CURVE('',#3670,#3668,#2202,.T.);
#4345=EDGE_CURVE('',#3669,#3670,#2203,.T.);
#4346=EDGE_CURVE('',#3664,#3669,#2204,.T.);
#4347=EDGE_CURVE('',#3665,#3670,#2205,.T.);
#4348=EDGE_CURVE('',#3671,#3672,#2206,.T.);
#4349=EDGE_CURVE('',#3672,#3673,#2207,.T.);
#4350=EDGE_CURVE('',#3674,#3673,#2208,.T.);
#4351=EDGE_CURVE('',#3671,#3674,#2209,.T.);
#4352=EDGE_CURVE('',#3675,#3671,#2210,.T.);
#4353=EDGE_CURVE('',#3676,#3674,#2211,.T.);
#4354=EDGE_CURVE('',#3675,#3676,#2212,.T.);
#4355=EDGE_CURVE('',#3677,#3675,#2213,.T.);
#4356=EDGE_CURVE('',#3678,#3676,#2214,.T.);
#4357=EDGE_CURVE('',#3677,#3678,#2215,.T.);
#4358=EDGE_CURVE('',#3672,#3677,#2216,.T.);
#4359=EDGE_CURVE('',#3673,#3678,#2217,.T.);
#4360=EDGE_CURVE('',#3679,#3680,#366,.T.);
#4361=EDGE_CURVE('',#3680,#3679,#367,.T.);
#4362=EDGE_CURVE('',#3680,#3681,#2218,.T.);
#4363=EDGE_CURVE('',#3682,#3681,#368,.T.);
#4364=EDGE_CURVE('',#3681,#3682,#369,.T.);
#4365=EDGE_CURVE('',#3683,#3683,#3240,.T.);
#4366=EDGE_CURVE('',#3683,#3684,#2219,.T.);
#4367=EDGE_CURVE('',#3684,#3684,#3241,.T.);
#4368=EDGE_CURVE('',#3685,#3685,#3242,.T.);
#4369=EDGE_CURVE('',#3685,#3686,#2220,.T.);
#4370=EDGE_CURVE('',#3686,#3686,#3243,.T.);
#4371=EDGE_CURVE('',#3687,#3687,#3244,.T.);
#4372=EDGE_CURVE('',#3687,#3688,#2221,.T.);
#4373=EDGE_CURVE('',#3688,#3688,#3245,.T.);
#4374=EDGE_CURVE('',#3689,#3689,#3246,.T.);
#4375=EDGE_CURVE('',#3689,#3690,#2222,.T.);
#4376=EDGE_CURVE('',#3690,#3690,#3247,.T.);
#4377=EDGE_CURVE('',#3691,#3692,#2223,.T.);
#4378=EDGE_CURVE('',#3691,#3693,#3248,.T.);
#4379=EDGE_CURVE('',#3694,#3693,#2224,.T.);
#4380=EDGE_CURVE('',#3692,#3694,#3249,.T.);
#4381=EDGE_CURVE('',#3693,#3691,#3250,.T.);
#4382=EDGE_CURVE('',#3695,#3696,#2225,.T.);
#4383=EDGE_CURVE('',#3695,#3697,#3251,.T.);
#4384=EDGE_CURVE('',#3698,#3697,#2226,.T.);
#4385=EDGE_CURVE('',#3696,#3698,#3252,.T.);
#4386=EDGE_CURVE('',#3697,#3695,#3253,.T.);
#4387=EDGE_CURVE('',#3699,#3700,#2227,.T.);
#4388=EDGE_CURVE('',#3699,#3701,#3254,.T.);
#4389=EDGE_CURVE('',#3702,#3701,#2228,.T.);
#4390=EDGE_CURVE('',#3700,#3702,#3255,.T.);
#4391=EDGE_CURVE('',#3701,#3699,#3256,.T.);
#4392=EDGE_CURVE('',#3703,#3704,#2229,.T.);
#4393=EDGE_CURVE('',#3703,#3705,#3257,.T.);
#4394=EDGE_CURVE('',#3706,#3705,#2230,.T.);
#4395=EDGE_CURVE('',#3704,#3706,#3258,.T.);
#4396=EDGE_CURVE('',#3705,#3703,#3259,.T.);
#4397=EDGE_CURVE('',#3707,#3707,#3260,.T.);
#4398=EDGE_CURVE('',#3696,#3708,#3261,.T.);
#4399=EDGE_CURVE('',#3700,#3698,#3262,.T.);
#4400=EDGE_CURVE('',#3704,#3702,#3263,.T.);
#4401=EDGE_CURVE('',#3692,#3706,#3264,.T.);
#4402=EDGE_CURVE('',#3708,#3694,#3265,.T.);
#4403=EDGE_CURVE('',#3709,#3709,#3266,.T.);
#4404=EDGE_CURVE('',#3710,#3710,#3267,.T.);
#4405=EDGE_CURVE('',#3711,#3711,#3268,.T.);
#4406=EDGE_CURVE('',#3712,#3712,#3269,.T.);
#4407=EDGE_CURVE('',#3713,#3713,#3270,.T.);
#4408=EDGE_CURVE('',#3713,#3709,#2231,.T.);
#4409=EDGE_CURVE('',#3714,#3714,#3271,.T.);
#4410=EDGE_CURVE('',#3714,#3710,#2232,.T.);
#4411=EDGE_CURVE('',#3715,#3715,#3272,.T.);
#4412=EDGE_CURVE('',#3715,#3711,#2233,.T.);
#4413=EDGE_CURVE('',#3716,#3716,#3273,.T.);
#4414=EDGE_CURVE('',#3716,#3712,#2234,.T.);
#4415=EDGE_CURVE('',#3717,#3717,#3274,.T.);
#4416=EDGE_CURVE('',#3717,#3708,#2235,.T.);
#4417=EDGE_CURVE('',#3718,#3718,#3275,.T.);
#4418=EDGE_CURVE('',#3718,#3719,#2236,.T.);
#4419=EDGE_CURVE('',#3719,#3719,#3276,.T.);
#4420=EDGE_CURVE('',#3720,#3720,#3277,.T.);
#4421=EDGE_CURVE('',#3707,#3721,#2237,.T.);
#4422=EDGE_CURVE('',#3721,#3721,#3278,.T.);
#4423=EDGE_CURVE('',#3720,#3722,#2238,.T.);
#4424=EDGE_CURVE('',#3722,#3722,#3279,.T.);
#4425=EDGE_CURVE('',#3723,#3723,#3280,.T.);
#4426=EDGE_CURVE('',#3723,#3724,#2239,.T.);
#4427=EDGE_CURVE('',#3724,#3724,#3281,.T.);
#4428=EDGE_CURVE('',#3725,#3725,#3282,.T.);
#4429=EDGE_CURVE('',#3726,#3726,#3283,.T.);
#4430=EDGE_CURVE('',#3726,#3727,#2240,.T.);
#4431=EDGE_CURVE('',#3727,#3727,#3284,.T.);
#4432=EDGE_CURVE('',#3728,#3728,#3285,.T.);
#4433=EDGE_CURVE('',#3729,#3729,#3286,.T.);
#4434=EDGE_CURVE('',#3729,#3730,#2241,.T.);
#4435=EDGE_CURVE('',#3730,#3730,#3287,.T.);
#4436=EDGE_CURVE('',#3731,#3731,#3288,.T.);
#4437=EDGE_CURVE('',#3732,#3732,#3289,.T.);
#4438=EDGE_CURVE('',#3732,#3733,#2242,.T.);
#4439=EDGE_CURVE('',#3733,#3733,#3290,.T.);
#4440=EDGE_CURVE('',#3734,#3734,#3291,.T.);
#4441=EDGE_CURVE('',#3735,#3735,#3292,.T.);
#4442=EDGE_CURVE('',#3735,#3725,#2243,.T.);
#4443=EDGE_CURVE('',#3736,#3736,#3293,.T.);
#4444=EDGE_CURVE('',#3736,#3728,#2244,.T.);
#4445=EDGE_CURVE('',#3737,#3737,#3294,.T.);
#4446=EDGE_CURVE('',#3737,#3731,#2245,.T.);
#4447=EDGE_CURVE('',#3738,#3738,#3295,.T.);
#4448=EDGE_CURVE('',#3738,#3734,#2246,.T.);
#4449=EDGE_CURVE('',#3739,#3739,#3296,.T.);
#4450=EDGE_CURVE('',#3739,#3740,#2247,.T.);
#4451=EDGE_CURVE('',#3740,#3740,#3297,.T.);
#4452=EDGE_CURVE('',#3741,#3741,#3298,.T.);
#4453=EDGE_CURVE('',#3742,#3742,#3299,.T.);
#4454=EDGE_CURVE('',#3742,#3741,#2248,.T.);
#4455=EDGE_CURVE('',#3743,#3743,#3300,.T.);
#4456=EDGE_CURVE('',#3743,#3744,#2249,.T.);
#4457=EDGE_CURVE('',#3744,#3744,#3301,.T.);
#4458=EDGE_CURVE('',#3745,#3746,#370,.T.);
#4459=EDGE_CURVE('',#3746,#3745,#371,.T.);
#4460=EDGE_CURVE('',#3746,#3747,#2250,.T.);
#4461=EDGE_CURVE('',#3748,#3747,#372,.T.);
#4462=EDGE_CURVE('',#3747,#3748,#373,.T.);
#4463=EDGE_CURVE('',#3749,#3749,#3302,.T.);
#4464=EDGE_CURVE('',#3749,#3750,#2251,.T.);
#4465=EDGE_CURVE('',#3750,#3750,#3303,.T.);
#4466=EDGE_CURVE('',#3751,#3751,#3304,.T.);
#4467=EDGE_CURVE('',#3751,#3752,#2252,.T.);
#4468=EDGE_CURVE('',#3752,#3752,#3305,.T.);
#4469=EDGE_CURVE('',#3753,#3753,#3306,.T.);
#4470=EDGE_CURVE('',#3753,#3754,#2253,.T.);
#4471=EDGE_CURVE('',#3754,#3754,#3307,.T.);
#4472=EDGE_CURVE('',#3755,#3755,#3308,.T.);
#4473=EDGE_CURVE('',#3755,#3756,#2254,.T.);
#4474=EDGE_CURVE('',#3756,#3756,#3309,.T.);
#4475=EDGE_CURVE('',#3757,#3758,#2255,.T.);
#4476=EDGE_CURVE('',#3757,#3759,#3310,.T.);
#4477=EDGE_CURVE('',#3760,#3759,#2256,.T.);
#4478=EDGE_CURVE('',#3758,#3760,#3311,.T.);
#4479=EDGE_CURVE('',#3759,#3757,#3312,.T.);
#4480=EDGE_CURVE('',#3761,#3762,#2257,.T.);
#4481=EDGE_CURVE('',#3761,#3763,#3313,.T.);
#4482=EDGE_CURVE('',#3764,#3763,#2258,.T.);
#4483=EDGE_CURVE('',#3762,#3764,#3314,.T.);
#4484=EDGE_CURVE('',#3763,#3761,#3315,.T.);
#4485=EDGE_CURVE('',#3765,#3766,#2259,.T.);
#4486=EDGE_CURVE('',#3765,#3767,#3316,.T.);
#4487=EDGE_CURVE('',#3768,#3767,#2260,.T.);
#4488=EDGE_CURVE('',#3766,#3768,#3317,.T.);
#4489=EDGE_CURVE('',#3767,#3765,#3318,.T.);
#4490=EDGE_CURVE('',#3769,#3770,#2261,.T.);
#4491=EDGE_CURVE('',#3769,#3771,#3319,.T.);
#4492=EDGE_CURVE('',#3772,#3771,#2262,.T.);
#4493=EDGE_CURVE('',#3770,#3772,#3320,.T.);
#4494=EDGE_CURVE('',#3771,#3769,#3321,.T.);
#4495=EDGE_CURVE('',#3773,#3773,#3322,.T.);
#4496=EDGE_CURVE('',#3762,#3774,#3323,.T.);
#4497=EDGE_CURVE('',#3766,#3764,#3324,.T.);
#4498=EDGE_CURVE('',#3770,#3768,#3325,.T.);
#4499=EDGE_CURVE('',#3758,#3772,#3326,.T.);
#4500=EDGE_CURVE('',#3774,#3760,#3327,.T.);
#4501=EDGE_CURVE('',#3775,#3775,#3328,.T.);
#4502=EDGE_CURVE('',#3776,#3776,#3329,.T.);
#4503=EDGE_CURVE('',#3777,#3777,#3330,.T.);
#4504=EDGE_CURVE('',#3778,#3778,#3331,.T.);
#4505=EDGE_CURVE('',#3779,#3779,#3332,.T.);
#4506=EDGE_CURVE('',#3779,#3775,#2263,.T.);
#4507=EDGE_CURVE('',#3780,#3780,#3333,.T.);
#4508=EDGE_CURVE('',#3780,#3776,#2264,.T.);
#4509=EDGE_CURVE('',#3781,#3781,#3334,.T.);
#4510=EDGE_CURVE('',#3781,#3777,#2265,.T.);
#4511=EDGE_CURVE('',#3782,#3782,#3335,.T.);
#4512=EDGE_CURVE('',#3782,#3778,#2266,.T.);
#4513=EDGE_CURVE('',#3783,#3783,#3336,.T.);
#4514=EDGE_CURVE('',#3783,#3774,#2267,.T.);
#4515=EDGE_CURVE('',#3784,#3784,#3337,.T.);
#4516=EDGE_CURVE('',#3784,#3785,#2268,.T.);
#4517=EDGE_CURVE('',#3785,#3785,#3338,.T.);
#4518=EDGE_CURVE('',#3786,#3786,#3339,.T.);
#4519=EDGE_CURVE('',#3773,#3787,#2269,.T.);
#4520=EDGE_CURVE('',#3787,#3787,#3340,.T.);
#4521=EDGE_CURVE('',#3786,#3788,#2270,.T.);
#4522=EDGE_CURVE('',#3788,#3788,#3341,.T.);
#4523=EDGE_CURVE('',#3789,#3789,#3342,.T.);
#4524=EDGE_CURVE('',#3789,#3790,#2271,.T.);
#4525=EDGE_CURVE('',#3790,#3790,#3343,.T.);
#4526=EDGE_CURVE('',#3791,#3791,#3344,.T.);
#4527=EDGE_CURVE('',#3792,#3792,#3345,.T.);
#4528=EDGE_CURVE('',#3792,#3793,#2272,.T.);
#4529=EDGE_CURVE('',#3793,#3793,#3346,.T.);
#4530=EDGE_CURVE('',#3794,#3794,#3347,.T.);
#4531=EDGE_CURVE('',#3795,#3795,#3348,.T.);
#4532=EDGE_CURVE('',#3795,#3796,#2273,.T.);
#4533=EDGE_CURVE('',#3796,#3796,#3349,.T.);
#4534=EDGE_CURVE('',#3797,#3797,#3350,.T.);
#4535=EDGE_CURVE('',#3798,#3798,#3351,.T.);
#4536=EDGE_CURVE('',#3798,#3799,#2274,.T.);
#4537=EDGE_CURVE('',#3799,#3799,#3352,.T.);
#4538=EDGE_CURVE('',#3800,#3800,#3353,.T.);
#4539=EDGE_CURVE('',#3801,#3801,#3354,.T.);
#4540=EDGE_CURVE('',#3801,#3791,#2275,.T.);
#4541=EDGE_CURVE('',#3802,#3802,#3355,.T.);
#4542=EDGE_CURVE('',#3802,#3794,#2276,.T.);
#4543=EDGE_CURVE('',#3803,#3803,#3356,.T.);
#4544=EDGE_CURVE('',#3803,#3797,#2277,.T.);
#4545=EDGE_CURVE('',#3804,#3804,#3357,.T.);
#4546=EDGE_CURVE('',#3804,#3800,#2278,.T.);
#4547=EDGE_CURVE('',#3805,#3805,#3358,.T.);
#4548=EDGE_CURVE('',#3805,#3806,#2279,.T.);
#4549=EDGE_CURVE('',#3806,#3806,#3359,.T.);
#4550=EDGE_CURVE('',#3807,#3807,#3360,.T.);
#4551=EDGE_CURVE('',#3808,#3808,#3361,.T.);
#4552=EDGE_CURVE('',#3808,#3807,#2280,.T.);
#4553=EDGE_CURVE('',#3809,#3809,#3362,.T.);
#4554=EDGE_CURVE('',#3809,#3810,#2281,.T.);
#4555=EDGE_CURVE('',#3810,#3810,#3363,.T.);
#4556=EDGE_CURVE('',#3811,#3811,#3364,.T.);
#4557=EDGE_CURVE('',#3811,#3812,#2282,.T.);
#4558=EDGE_CURVE('',#3812,#3812,#3365,.T.);
#4559=EDGE_CURVE('',#3813,#3813,#3366,.T.);
#4560=EDGE_CURVE('',#3814,#3814,#3367,.T.);
#4561=EDGE_CURVE('',#3814,#3815,#2283,.T.);
#4562=EDGE_CURVE('',#3815,#3815,#3368,.T.);
#4563=EDGE_CURVE('',#3816,#3816,#3369,.T.);
#4564=EDGE_CURVE('',#3817,#3817,#3370,.T.);
#4565=EDGE_CURVE('',#3817,#3818,#2284,.T.);
#4566=EDGE_CURVE('',#3818,#3818,#3371,.T.);
#4567=EDGE_CURVE('',#3819,#3819,#3372,.T.);
#4568=EDGE_CURVE('',#3820,#3820,#3373,.T.);
#4569=EDGE_CURVE('',#3820,#3821,#2285,.T.);
#4570=EDGE_CURVE('',#3821,#3821,#3374,.T.);
#4571=EDGE_CURVE('',#3822,#3822,#3375,.T.);
#4572=EDGE_CURVE('',#3823,#3823,#3376,.T.);
#4573=EDGE_CURVE('',#3823,#3813,#2286,.T.);
#4574=EDGE_CURVE('',#3824,#3824,#3377,.T.);
#4575=EDGE_CURVE('',#3824,#3816,#2287,.T.);
#4576=EDGE_CURVE('',#3825,#3825,#3378,.T.);
#4577=EDGE_CURVE('',#3825,#3819,#2288,.T.);
#4578=EDGE_CURVE('',#3826,#3826,#3379,.T.);
#4579=EDGE_CURVE('',#3826,#3822,#2289,.T.);
#4580=EDGE_CURVE('',#3827,#3828,#2290,.T.);
#4581=EDGE_CURVE('',#3828,#3829,#2291,.T.);
#4582=EDGE_CURVE('',#3830,#3829,#2292,.T.);
#4583=EDGE_CURVE('',#3827,#3830,#2293,.T.);
#4584=EDGE_CURVE('',#3831,#3827,#2294,.T.);
#4585=EDGE_CURVE('',#3832,#3830,#2295,.T.);
#4586=EDGE_CURVE('',#3831,#3832,#2296,.T.);
#4587=EDGE_CURVE('',#3833,#3831,#2297,.T.);
#4588=EDGE_CURVE('',#3834,#3832,#2298,.T.);
#4589=EDGE_CURVE('',#3833,#3834,#2299,.T.);
#4590=EDGE_CURVE('',#3835,#3833,#2300,.T.);
#4591=EDGE_CURVE('',#3836,#3834,#2301,.T.);
#4592=EDGE_CURVE('',#3835,#3836,#2302,.T.);
#4593=EDGE_CURVE('',#3837,#3835,#2303,.T.);
#4594=EDGE_CURVE('',#3838,#3836,#2304,.T.);
#4595=EDGE_CURVE('',#3837,#3838,#2305,.T.);
#4596=EDGE_CURVE('',#3839,#3837,#2306,.T.);
#4597=EDGE_CURVE('',#3840,#3838,#2307,.T.);
#4598=EDGE_CURVE('',#3839,#3840,#2308,.T.);
#4599=EDGE_CURVE('',#3841,#3839,#2309,.T.);
#4600=EDGE_CURVE('',#3842,#3840,#2310,.T.);
#4601=EDGE_CURVE('',#3841,#3842,#2311,.T.);
#4602=EDGE_CURVE('',#3843,#3841,#2312,.T.);
#4603=EDGE_CURVE('',#3844,#3842,#2313,.T.);
#4604=EDGE_CURVE('',#3843,#3844,#2314,.T.);
#4605=EDGE_CURVE('',#3845,#3843,#2315,.T.);
#4606=EDGE_CURVE('',#3846,#3844,#2316,.T.);
#4607=EDGE_CURVE('',#3845,#3846,#2317,.T.);
#4608=EDGE_CURVE('',#3847,#3845,#2318,.T.);
#4609=EDGE_CURVE('',#3848,#3846,#2319,.T.);
#4610=EDGE_CURVE('',#3847,#3848,#2320,.T.);
#4611=EDGE_CURVE('',#3849,#3847,#2321,.T.);
#4612=EDGE_CURVE('',#3850,#3848,#2322,.T.);
#4613=EDGE_CURVE('',#3849,#3850,#2323,.T.);
#4614=EDGE_CURVE('',#3828,#3849,#2324,.T.);
#4615=EDGE_CURVE('',#3829,#3850,#2325,.T.);
#4616=EDGE_CURVE('',#3851,#3852,#3380,.T.);
#4617=EDGE_CURVE('',#3852,#3851,#3381,.T.);
#4618=EDGE_CURVE('',#3852,#3853,#3382,.T.);
#4619=EDGE_CURVE('',#3854,#3853,#3383,.T.);
#4620=EDGE_CURVE('',#3853,#3854,#3384,.T.);
#4621=EDGE_CURVE('',#3854,#3855,#2326,.T.);
#4622=EDGE_CURVE('',#3855,#3855,#3385,.T.);
#4623=EDGE_CURVE('',#3856,#3856,#3386,.T.);
#4624=EDGE_CURVE('',#3856,#3857,#2327,.T.);
#4625=EDGE_CURVE('',#3857,#3857,#3387,.T.);
#4626=EDGE_CURVE('',#3857,#3858,#2328,.T.);
#4627=EDGE_CURVE('',#3858,#3858,#3388,.T.);
#4628=EDGE_CURVE('',#3859,#3859,#3389,.T.);
#4629=EDGE_CURVE('',#3859,#3851,#2329,.T.);
#4630=EDGE_CURVE('',#3860,#3860,#3390,.T.);
#4631=EDGE_CURVE('',#3860,#3856,#2330,.T.);
#4632=EDGE_CURVE('',#3861,#3862,#3391,.T.);
#4633=EDGE_CURVE('',#3862,#3861,#3392,.T.);
#4634=EDGE_CURVE('',#3862,#3863,#3393,.T.);
#4635=EDGE_CURVE('',#3864,#3863,#3394,.T.);
#4636=EDGE_CURVE('',#3863,#3864,#3395,.T.);
#4637=EDGE_CURVE('',#3865,#3865,#3396,.T.);
#4638=EDGE_CURVE('',#3865,#3864,#2331,.T.);
#4639=EDGE_CURVE('',#3866,#3866,#3397,.T.);
#4640=EDGE_CURVE('',#3867,#3867,#3398,.T.);
#4641=EDGE_CURVE('',#3868,#3868,#3399,.T.);
#4642=EDGE_CURVE('',#3868,#3866,#2332,.T.);
#4643=EDGE_CURVE('',#3869,#3869,#3400,.T.);
#4644=EDGE_CURVE('',#3869,#3868,#2333,.T.);
#4645=EDGE_CURVE('',#3870,#3870,#3401,.T.);
#4646=EDGE_CURVE('',#3870,#3869,#2334,.T.);
#4647=EDGE_CURVE('',#3861,#3867,#2335,.T.);
#4648=EDGE_CURVE('',#3871,#3872,#3402,.T.);
#4649=EDGE_CURVE('',#3873,#3874,#3403,.T.);
#4650=EDGE_CURVE('',#3875,#3876,#3404,.T.);
#4651=EDGE_CURVE('',#3877,#3878,#3405,.T.);
#4652=EDGE_CURVE('',#3879,#3880,#3406,.T.);
#4653=EDGE_CURVE('',#3881,#3882,#3407,.T.);
#4654=EDGE_CURVE('',#3883,#3884,#3408,.T.);
#4655=EDGE_CURVE('',#3885,#3886,#3409,.T.);
#4656=EDGE_CURVE('',#3887,#3888,#374,.T.);
#4657=EDGE_CURVE('',#3889,#3887,#3410,.T.);
#4658=EDGE_CURVE('',#3890,#3889,#375,.T.);
#4659=EDGE_CURVE('',#3888,#3890,#3411,.T.);
#4660=EDGE_CURVE('',#3891,#3889,#3412,.T.);
#4661=EDGE_CURVE('',#3891,#3892,#376,.T.);
#4662=EDGE_CURVE('',#3893,#3892,#3413,.T.);
#4663=EDGE_CURVE('',#3893,#3894,#377,.T.);
#4664=EDGE_CURVE('',#3895,#3894,#3414,.T.);
#4665=EDGE_CURVE('',#3895,#3896,#378,.T.);
#4666=EDGE_CURVE('',#3896,#3897,#2336,.T.);
#4667=EDGE_CURVE('',#3897,#3897,#3415,.T.);
#4668=EDGE_CURVE('',#3896,#3898,#379,.T.);
#4669=EDGE_CURVE('',#3899,#3898,#3416,.T.);
#4670=EDGE_CURVE('',#3899,#3900,#380,.T.);
#4671=EDGE_CURVE('',#3901,#3900,#3417,.T.);
#4672=EDGE_CURVE('',#3901,#3902,#381,.T.);
#4673=EDGE_CURVE('',#3903,#3902,#3418,.T.);
#4674=EDGE_CURVE('',#3903,#3904,#382,.T.);
#4675=EDGE_CURVE('',#3905,#3904,#3419,.T.);
#4676=EDGE_CURVE('',#3905,#3906,#383,.T.);
#4677=EDGE_CURVE('',#3890,#3906,#3420,.T.);
#4678=EDGE_CURVE('',#3887,#3907,#3421,.T.);
#4679=EDGE_CURVE('',#3907,#3891,#3422,.T.);
#4680=EDGE_CURVE('',#3908,#3907,#384,.T.);
#4681=EDGE_CURVE('',#3892,#3908,#3423,.T.);
#4682=EDGE_CURVE('',#3908,#3909,#3424,.T.);
#4683=EDGE_CURVE('',#3909,#3893,#3425,.T.);
#4684=EDGE_CURVE('',#3910,#3909,#385,.T.);
#4685=EDGE_CURVE('',#3894,#3910,#3426,.T.);
#4686=EDGE_CURVE('',#3910,#3911,#3427,.T.);
#4687=EDGE_CURVE('',#3911,#3895,#3428,.T.);
#4688=EDGE_CURVE('',#3912,#3913,#386,.T.);
#4689=EDGE_CURVE('',#3898,#3912,#3429,.T.);
#4690=EDGE_CURVE('',#3913,#3911,#387,.T.);
#4691=EDGE_CURVE('',#3912,#3914,#3430,.T.);
#4692=EDGE_CURVE('',#3914,#3899,#3431,.T.);
#4693=EDGE_CURVE('',#3915,#3914,#388,.T.);
#4694=EDGE_CURVE('',#3900,#3915,#3432,.T.);
#4695=EDGE_CURVE('',#3915,#3916,#3433,.T.);
#4696=EDGE_CURVE('',#3916,#3901,#3434,.T.);
#4697=EDGE_CURVE('',#3917,#3916,#389,.T.);
#4698=EDGE_CURVE('',#3902,#3917,#3435,.T.);
#4699=EDGE_CURVE('',#3917,#3918,#3436,.T.);
#4700=EDGE_CURVE('',#3918,#3903,#3437,.T.);
#4701=EDGE_CURVE('',#3919,#3918,#390,.T.);
#4702=EDGE_CURVE('',#3904,#3919,#3438,.T.);
#4703=EDGE_CURVE('',#3920,#3920,#3439,.T.);
#4704=EDGE_CURVE('',#3920,#3913,#2337,.T.);
#4705=EDGE_CURVE('',#3921,#3888,#3440,.T.);
#4706=EDGE_CURVE('',#3921,#3922,#391,.T.);
#4707=EDGE_CURVE('',#3919,#3922,#3441,.T.);
#4708=EDGE_CURVE('',#3906,#3921,#3442,.T.);
#4709=EDGE_CURVE('',#3922,#3905,#3443,.T.);
#4710=EDGE_CURVE('',#3923,#3923,#3444,.T.);
#4711=EDGE_CURVE('',#3924,#3924,#3445,.T.);
#4712=EDGE_CURVE('',#3925,#3925,#3446,.T.);
#4713=EDGE_CURVE('',#3925,#3923,#2338,.T.);
#4714=EDGE_CURVE('',#3926,#3926,#3447,.T.);
#4715=EDGE_CURVE('',#3926,#3924,#2339,.T.);
#4716=EDGE_CURVE('',#3927,#3927,#3448,.T.);
#4717=EDGE_CURVE('',#3928,#3928,#3449,.T.);
#4718=EDGE_CURVE('',#3929,#3929,#3450,.T.);
#4719=EDGE_CURVE('',#3929,#3927,#2340,.T.);
#4720=EDGE_CURVE('',#3930,#3930,#3451,.T.);
#4721=EDGE_CURVE('',#3930,#3928,#2341,.T.);
#4722=EDGE_CURVE('',#3931,#3931,#3452,.T.);
#4723=EDGE_CURVE('',#3931,#3932,#2342,.T.);
#4724=EDGE_CURVE('',#3932,#3932,#3453,.T.);
#4725=EDGE_CURVE('',#3933,#3934,#2343,.T.);
#4726=EDGE_CURVE('',#3935,#3933,#3454,.T.);
#4727=EDGE_CURVE('',#3936,#3935,#2344,.T.);
#4728=EDGE_CURVE('',#3936,#3934,#3455,.T.);
#4729=EDGE_CURVE('',#3937,#3934,#2345,.T.);
#4730=EDGE_CURVE('',#3938,#3937,#2346,.T.);
#4731=EDGE_CURVE('',#3933,#3938,#2347,.T.);
#4732=EDGE_CURVE('',#3936,#3939,#2348,.T.);
#4733=EDGE_CURVE('',#3940,#3939,#3456,.T.);
#4734=EDGE_CURVE('',#3940,#3941,#2349,.T.);
#4735=EDGE_CURVE('',#3942,#3941,#3457,.T.);
#4736=EDGE_CURVE('',#3942,#3943,#2350,.T.);
#4737=EDGE_CURVE('',#3937,#3943,#3458,.T.);
#4738=EDGE_CURVE('',#3944,#3944,#3459,.T.);
#4739=EDGE_CURVE('',#3945,#3945,#3460,.T.);
#4740=EDGE_CURVE('',#3946,#3935,#2351,.T.);
#4741=EDGE_CURVE('',#3939,#3946,#2352,.T.);
#4742=EDGE_CURVE('',#3947,#3946,#3461,.T.);
#4743=EDGE_CURVE('',#3947,#3940,#2353,.T.);
#4744=EDGE_CURVE('',#3944,#3948,#2354,.T.);
#4745=EDGE_CURVE('',#3948,#3948,#3462,.T.);
#4746=EDGE_CURVE('',#3942,#3949,#2355,.T.);
#4747=EDGE_CURVE('',#3950,#3941,#2356,.T.);
#4748=EDGE_CURVE('',#3949,#3950,#3463,.T.);
#4749=EDGE_CURVE('',#3951,#3949,#2357,.T.);
#4750=EDGE_CURVE('',#3943,#3951,#2358,.T.);
#4751=EDGE_CURVE('',#3938,#3951,#3464,.T.);
#4752=EDGE_CURVE('',#3950,#3947,#2359,.T.);
#4753=EDGE_CURVE('',#3952,#3952,#3465,.T.);
#4754=EDGE_CURVE('',#3953,#3953,#3466,.T.);
#4755=EDGE_CURVE('',#3945,#3952,#2360,.T.);
#4756=EDGE_CURVE('',#3953,#3954,#2361,.T.);
#4757=EDGE_CURVE('',#3954,#3954,#3467,.T.);
#4758=EDGE_CURVE('',#3955,#3955,#3468,.T.);
#4759=EDGE_CURVE('',#3955,#3956,#2362,.T.);
#4760=EDGE_CURVE('',#3956,#3956,#3469,.T.);
#4761=EDGE_CURVE('',#3957,#3957,#3470,.T.);
#4762=EDGE_CURVE('',#3957,#3958,#2363,.T.);
#4763=EDGE_CURVE('',#3958,#3958,#3471,.T.);
#4764=EDGE_CURVE('',#3959,#3959,#3472,.T.);
#4765=EDGE_CURVE('',#3959,#3960,#2364,.T.);
#4766=EDGE_CURVE('',#3960,#3960,#3473,.T.);
#4767=EDGE_CURVE('',#3961,#3961,#3474,.T.);
#4768=EDGE_CURVE('',#3961,#3962,#2365,.T.);
#4769=EDGE_CURVE('',#3962,#3962,#3475,.T.);
#4770=EDGE_CURVE('',#3963,#3964,#2366,.T.);
#4771=EDGE_CURVE('',#3963,#3964,#3476,.T.);
#4772=EDGE_CURVE('',#3965,#3963,#392,.T.);
#4773=EDGE_CURVE('',#3966,#3965,#3477,.T.);
#4774=EDGE_CURVE('',#3967,#3966,#393,.T.);
#4775=EDGE_CURVE('',#3967,#3968,#2367,.T.);
#4776=EDGE_CURVE('',#3969,#3968,#394,.T.);
#4777=EDGE_CURVE('',#3968,#3969,#395,.T.);
#4778=EDGE_CURVE('',#3964,#3967,#396,.T.);
#4779=EDGE_CURVE('',#3966,#3965,#2368,.T.);
#4780=EDGE_CURVE('',#3970,#3970,#3478,.T.);
#4781=EDGE_CURVE('',#3970,#3971,#2369,.T.);
#4782=EDGE_CURVE('',#3971,#3971,#3479,.T.);
#4783=EDGE_CURVE('',#3972,#3972,#3480,.T.);
#4784=EDGE_CURVE('',#3972,#3973,#2370,.T.);
#4785=EDGE_CURVE('',#3973,#3973,#3481,.T.);
#4786=EDGE_CURVE('',#3974,#3974,#3482,.T.);
#4787=EDGE_CURVE('',#3974,#3975,#2371,.T.);
#4788=EDGE_CURVE('',#3975,#3975,#3483,.T.);
#4789=EDGE_CURVE('',#3976,#3976,#3484,.T.);
#4790=EDGE_CURVE('',#3977,#3977,#3485,.T.);
#4791=EDGE_CURVE('',#3978,#3978,#3486,.T.);
#4792=EDGE_CURVE('',#3979,#3979,#3487,.T.);
#4793=EDGE_CURVE('',#3976,#3978,#2372,.T.);
#4794=EDGE_CURVE('',#3979,#3980,#2373,.T.);
#4795=EDGE_CURVE('',#3980,#3980,#3488,.T.);
#4796=EDGE_CURVE('',#3981,#3981,#3489,.T.);
#4797=EDGE_CURVE('',#3981,#3977,#2374,.T.);
#4798=EDGE_CURVE('',#3982,#3982,#3490,.T.);
#4799=EDGE_CURVE('',#3982,#3983,#2375,.T.);
#4800=EDGE_CURVE('',#3983,#3983,#3491,.T.);
#4801=EDGE_CURVE('',#3984,#3984,#3492,.T.);
#4802=EDGE_CURVE('',#3984,#3985,#2376,.T.);
#4803=EDGE_CURVE('',#3985,#3985,#3493,.T.);
#4804=EDGE_CURVE('',#3986,#3986,#3494,.T.);
#4805=EDGE_CURVE('',#3986,#3987,#2377,.T.);
#4806=EDGE_CURVE('',#3987,#3987,#3495,.T.);
#4807=EDGE_CURVE('',#3988,#3988,#3496,.T.);
#4808=EDGE_CURVE('',#3988,#3989,#2378,.T.);
#4809=EDGE_CURVE('',#3989,#3989,#3497,.T.);
#4810=EDGE_CURVE('',#3990,#3990,#3498,.T.);
#4811=EDGE_CURVE('',#3990,#3991,#2379,.T.);
#4812=EDGE_CURVE('',#3991,#3991,#3499,.T.);
#4813=EDGE_CURVE('',#3992,#3992,#3500,.T.);
#4814=EDGE_CURVE('',#3992,#3993,#2380,.T.);
#4815=EDGE_CURVE('',#3993,#3993,#3501,.T.);
#4816=EDGE_CURVE('',#3994,#3994,#3502,.T.);
#4817=EDGE_CURVE('',#3995,#3995,#3503,.T.);
#4818=EDGE_CURVE('',#3995,#3994,#2381,.T.);
#4819=EDGE_CURVE('',#3996,#3996,#3504,.T.);
#4820=EDGE_CURVE('',#3996,#3995,#2382,.T.);
#4821=EDGE_CURVE('',#3997,#3997,#3505,.T.);
#4822=EDGE_CURVE('',#3997,#3996,#2383,.T.);
#4823=EDGE_CURVE('',#3998,#3998,#3506,.T.);
#4824=EDGE_CURVE('',#3999,#3999,#3507,.F.);
#4825=EDGE_CURVE('',#3999,#3998,#2384,.T.);
#4826=EDGE_CURVE('',#4000,#4000,#3508,.F.);
#4827=EDGE_CURVE('',#4000,#3999,#2385,.T.);
#4828=EDGE_CURVE('',#4001,#4001,#3509,.T.);
#4829=EDGE_CURVE('',#4001,#4000,#2386,.T.);
#4830=EDGE_CURVE('',#4002,#4003,#2387,.T.);
#4831=EDGE_CURVE('',#4003,#4004,#2388,.T.);
#4832=EDGE_CURVE('',#4004,#4005,#2389,.T.);
#4833=EDGE_CURVE('',#4002,#4005,#2390,.T.);
#4834=EDGE_CURVE('',#4003,#4006,#2391,.T.);
#4835=EDGE_CURVE('',#4006,#4007,#2392,.T.);
#4836=EDGE_CURVE('',#4007,#4004,#2393,.T.);
#4837=EDGE_CURVE('',#4006,#4008,#2394,.T.);
#4838=EDGE_CURVE('',#4008,#4009,#2395,.T.);
#4839=EDGE_CURVE('',#4009,#4007,#2396,.T.);
#4840=EDGE_CURVE('',#4008,#4010,#2397,.T.);
#4841=EDGE_CURVE('',#4010,#4011,#2398,.T.);
#4842=EDGE_CURVE('',#4011,#4009,#2399,.T.);
#4843=EDGE_CURVE('',#4010,#4012,#2400,.T.);
#4844=EDGE_CURVE('',#4012,#4013,#2401,.T.);
#4845=EDGE_CURVE('',#4013,#4011,#2402,.T.);
#4846=EDGE_CURVE('',#4012,#4002,#2403,.T.);
#4847=EDGE_CURVE('',#4005,#4013,#2404,.T.);
#4848=EDGE_CURVE('',#4014,#4014,#3510,.T.);
#4849=EDGE_CURVE('',#4014,#4015,#2405,.T.);
#4850=EDGE_CURVE('',#4015,#4015,#3511,.T.);
#4851=EDGE_CURVE('',#4016,#4017,#2406,.T.);
#4852=EDGE_CURVE('',#4016,#4018,#2407,.T.);
#4853=EDGE_CURVE('',#4019,#4018,#2408,.T.);
#4854=EDGE_CURVE('',#4017,#4019,#2409,.T.);
#4855=EDGE_CURVE('',#4017,#4020,#2410,.T.);
#4856=EDGE_CURVE('',#4021,#4019,#2411,.T.);
#4857=EDGE_CURVE('',#4020,#4021,#2412,.T.);
#4858=EDGE_CURVE('',#4020,#4022,#2413,.T.);
#4859=EDGE_CURVE('',#4023,#4021,#2414,.T.);
#4860=EDGE_CURVE('',#4022,#4023,#2415,.T.);
#4861=EDGE_CURVE('',#4022,#4016,#2416,.T.);
#4862=EDGE_CURVE('',#4018,#4023,#2417,.T.);
#4863=EDGE_CURVE('',#4024,#4025,#2418,.T.);
#4864=EDGE_CURVE('',#4026,#4025,#3512,.T.);
#4865=EDGE_CURVE('',#4027,#4026,#2419,.T.);
#4866=EDGE_CURVE('',#4027,#4024,#3513,.T.);
#4867=EDGE_CURVE('',#4027,#4028,#2420,.T.);
#4868=EDGE_CURVE('',#4029,#4028,#3514,.T.);
#4869=EDGE_CURVE('',#4029,#4024,#2421,.T.);
#4870=EDGE_CURVE('',#4030,#4030,#3515,.T.);
#4871=EDGE_CURVE('',#4031,#4029,#2422,.T.);
#4872=EDGE_CURVE('',#4025,#4031,#2423,.T.);
#4873=EDGE_CURVE('',#4032,#4026,#2424,.T.);
#4874=EDGE_CURVE('',#4028,#4032,#2425,.T.);
#4875=EDGE_CURVE('',#4031,#4032,#3516,.T.);
#4876=EDGE_CURVE('',#4033,#4033,#3517,.T.);
#4877=EDGE_CURVE('',#4034,#4034,#3518,.T.);
#4878=EDGE_CURVE('',#4030,#4033,#2426,.T.);
#4879=EDGE_CURVE('',#4034,#4035,#2427,.T.);
#4880=EDGE_CURVE('',#4035,#4035,#3519,.T.);
#4881=EDGE_CURVE('',#4036,#4036,#3520,.T.);
#4882=EDGE_CURVE('',#4036,#4037,#2428,.T.);
#4883=EDGE_CURVE('',#4037,#4037,#3521,.T.);
#4884=EDGE_CURVE('',#4038,#4038,#3522,.T.);
#4885=EDGE_CURVE('',#4038,#4039,#2429,.T.);
#4886=EDGE_CURVE('',#4039,#4039,#3523,.T.);
#4887=EDGE_CURVE('',#4040,#4041,#2430,.T.);
#4888=EDGE_CURVE('',#4040,#4041,#3524,.T.);
#4889=EDGE_CURVE('',#4042,#4040,#397,.T.);
#4890=EDGE_CURVE('',#4043,#4042,#3525,.T.);
#4891=EDGE_CURVE('',#4044,#4043,#398,.T.);
#4892=EDGE_CURVE('',#4044,#4045,#2431,.T.);
#4893=EDGE_CURVE('',#4046,#4045,#399,.T.);
#4894=EDGE_CURVE('',#4045,#4046,#400,.T.);
#4895=EDGE_CURVE('',#4041,#4044,#401,.T.);
#4896=EDGE_CURVE('',#4043,#4042,#2432,.T.);
#4897=EDGE_CURVE('',#4047,#4047,#3526,.T.);
#4898=EDGE_CURVE('',#4047,#4048,#2433,.T.);
#4899=EDGE_CURVE('',#4048,#4048,#3527,.T.);
#4900=EDGE_CURVE('',#4049,#4049,#3528,.T.);
#4901=EDGE_CURVE('',#4049,#4050,#2434,.T.);
#4902=EDGE_CURVE('',#4050,#4050,#3529,.T.);
#4903=EDGE_CURVE('',#4051,#4051,#3530,.T.);
#4904=EDGE_CURVE('',#4051,#4052,#2435,.T.);
#4905=EDGE_CURVE('',#4052,#4052,#3531,.T.);
#4906=EDGE_CURVE('',#4053,#4053,#3532,.T.);
#4907=EDGE_CURVE('',#4054,#4054,#3533,.T.);
#4908=EDGE_CURVE('',#4055,#4055,#3534,.T.);
#4909=EDGE_CURVE('',#4056,#4056,#3535,.T.);
#4910=EDGE_CURVE('',#4053,#4055,#2436,.T.);
#4911=EDGE_CURVE('',#4056,#4057,#2437,.T.);
#4912=EDGE_CURVE('',#4057,#4057,#3536,.T.);
#4913=EDGE_CURVE('',#4058,#4058,#3537,.T.);
#4914=EDGE_CURVE('',#4058,#4054,#2438,.T.);
#4915=EDGE_CURVE('',#4059,#4059,#3538,.T.);
#4916=EDGE_CURVE('',#4059,#4060,#2439,.T.);
#4917=EDGE_CURVE('',#4060,#4060,#3539,.T.);
#4918=EDGE_CURVE('',#4061,#4061,#3540,.T.);
#4919=EDGE_CURVE('',#4061,#4062,#2440,.T.);
#4920=EDGE_CURVE('',#4062,#4062,#3541,.T.);
#4921=EDGE_CURVE('',#4063,#4063,#3542,.T.);
#4922=EDGE_CURVE('',#4063,#4064,#2441,.T.);
#4923=EDGE_CURVE('',#4064,#4064,#3543,.T.);
#4924=EDGE_CURVE('',#4065,#4065,#3544,.T.);
#4925=EDGE_CURVE('',#4065,#4066,#2442,.T.);
#4926=EDGE_CURVE('',#4066,#4066,#3545,.T.);
#4927=EDGE_CURVE('',#4067,#4067,#3546,.T.);
#4928=EDGE_CURVE('',#4067,#4068,#2443,.T.);
#4929=EDGE_CURVE('',#4068,#4068,#3547,.T.);
#4930=EDGE_CURVE('',#4069,#4069,#3548,.T.);
#4931=EDGE_CURVE('',#4069,#4070,#2444,.T.);
#4932=EDGE_CURVE('',#4070,#4070,#3549,.T.);
#4933=EDGE_CURVE('',#4071,#4071,#3550,.T.);
#4934=EDGE_CURVE('',#4072,#4073,#2445,.T.);
#4935=EDGE_CURVE('',#4072,#4074,#2446,.T.);
#4936=EDGE_CURVE('',#4074,#4075,#2447,.T.);
#4937=EDGE_CURVE('',#4073,#4075,#2448,.T.);
#4938=EDGE_CURVE('',#4076,#4072,#2449,.T.);
#4939=EDGE_CURVE('',#4076,#4077,#2450,.T.);
#4940=EDGE_CURVE('',#4077,#4074,#2451,.T.);
#4941=EDGE_CURVE('',#4078,#4076,#2452,.T.);
#4942=EDGE_CURVE('',#4078,#4079,#2453,.T.);
#4943=EDGE_CURVE('',#4079,#4077,#2454,.T.);
#4944=EDGE_CURVE('',#4080,#4078,#2455,.T.);
#4945=EDGE_CURVE('',#4080,#4081,#2456,.T.);
#4946=EDGE_CURVE('',#4081,#4079,#2457,.T.);
#4947=EDGE_CURVE('',#4082,#4080,#2458,.T.);
#4948=EDGE_CURVE('',#4082,#4083,#2459,.T.);
#4949=EDGE_CURVE('',#4083,#4081,#2460,.T.);
#4950=EDGE_CURVE('',#4073,#4082,#2461,.T.);
#4951=EDGE_CURVE('',#4075,#4083,#2462,.T.);
#4952=EDGE_CURVE('',#4084,#4084,#3551,.T.);
#4953=EDGE_CURVE('',#4085,#4085,#3552,.T.);
#4954=EDGE_CURVE('',#4085,#4084,#2463,.T.);
#4955=EDGE_CURVE('',#4071,#4085,#2464,.T.);
#4956=EDGE_CURVE('',#4086,#4086,#3553,.T.);
#4957=EDGE_CURVE('',#4086,#4087,#2465,.T.);
#4958=EDGE_CURVE('',#4087,#4087,#3554,.T.);
#4959=EDGE_CURVE('',#4088,#4089,#2466,.T.);
#4960=EDGE_CURVE('',#4090,#4089,#2467,.T.);
#4961=EDGE_CURVE('',#4091,#4090,#2468,.T.);
#4962=EDGE_CURVE('',#4088,#4091,#2469,.T.);
#4963=EDGE_CURVE('',#4092,#4093,#2470,.T.);
#4964=EDGE_CURVE('',#4094,#4093,#2471,.T.);
#4965=EDGE_CURVE('',#4095,#4094,#2472,.T.);
#4966=EDGE_CURVE('',#4092,#4095,#2473,.T.);
#4967=EDGE_CURVE('',#4090,#4096,#2474,.T.);
#4968=EDGE_CURVE('',#4097,#4096,#2475,.T.);
#4969=EDGE_CURVE('',#4091,#4097,#2476,.T.);
#4970=EDGE_CURVE('',#4094,#4098,#2477,.T.);
#4971=EDGE_CURVE('',#4099,#4098,#2478,.T.);
#4972=EDGE_CURVE('',#4095,#4099,#2479,.T.);
#4973=EDGE_CURVE('',#4098,#4097,#2480,.T.);
#4974=EDGE_CURVE('',#4096,#4099,#2481,.T.);
#4975=EDGE_CURVE('',#4100,#4101,#2482,.T.);
#4976=EDGE_CURVE('',#4100,#4102,#2483,.T.);
#4977=EDGE_CURVE('',#4102,#4103,#2484,.T.);
#4978=EDGE_CURVE('',#4103,#4101,#2485,.T.);
#4979=EDGE_CURVE('',#4104,#4105,#2486,.T.);
#4980=EDGE_CURVE('',#4104,#4106,#2487,.T.);
#4981=EDGE_CURVE('',#4106,#4107,#2488,.T.);
#4982=EDGE_CURVE('',#4107,#4105,#2489,.T.);
#4983=EDGE_CURVE('',#4108,#4109,#2490,.T.);
#4984=EDGE_CURVE('',#4109,#4107,#2491,.T.);
#4985=EDGE_CURVE('',#4108,#4106,#2492,.T.);
#4986=EDGE_CURVE('',#4110,#4111,#2493,.T.);
#4987=EDGE_CURVE('',#4111,#4103,#2494,.T.);
#4988=EDGE_CURVE('',#4110,#4102,#2495,.T.);
#4989=EDGE_CURVE('',#4109,#4110,#2496,.T.);
#4990=EDGE_CURVE('',#4111,#4108,#2497,.T.);
#4991=EDGE_CURVE('',#4100,#4092,#2498,.T.);
#4992=EDGE_CURVE('',#4105,#4089,#2499,.T.);
#4993=EDGE_CURVE('',#4104,#4088,#2500,.T.);
#4994=EDGE_CURVE('',#4101,#4093,#2501,.T.);
#4995=EDGE_CURVE('',#4112,#4112,#3555,.T.);
#4996=EDGE_CURVE('',#4112,#4113,#2502,.T.);
#4997=EDGE_CURVE('',#4113,#4113,#3556,.T.);
#4998=EDGE_CURVE('',#4114,#4114,#3557,.T.);
#4999=EDGE_CURVE('',#4114,#4115,#2503,.T.);
#5000=EDGE_CURVE('',#4115,#4115,#3558,.T.);
#5001=EDGE_CURVE('',#4116,#4117,#2504,.T.);
#5002=EDGE_CURVE('',#4118,#4116,#3559,.T.);
#5003=EDGE_CURVE('',#4119,#4118,#2505,.T.);
#5004=EDGE_CURVE('',#4119,#4117,#3560,.T.);
#5005=EDGE_CURVE('',#4120,#4117,#2506,.T.);
#5006=EDGE_CURVE('',#4121,#4120,#2507,.T.);
#5007=EDGE_CURVE('',#4116,#4121,#2508,.T.);
#5008=EDGE_CURVE('',#4119,#4122,#2509,.T.);
#5009=EDGE_CURVE('',#4120,#4122,#3561,.T.);
#5010=EDGE_CURVE('',#4123,#4118,#2510,.T.);
#5011=EDGE_CURVE('',#4122,#4123,#2511,.T.);
#5012=EDGE_CURVE('',#4121,#4123,#3562,.T.);
#5013=EDGE_CURVE('',#4124,#4124,#3563,.T.);
#5014=EDGE_CURVE('',#4124,#4125,#2512,.T.);
#5015=EDGE_CURVE('',#4125,#4125,#3564,.T.);
#5016=EDGE_CURVE('',#4126,#4126,#3565,.T.);
#5017=EDGE_CURVE('',#4126,#4127,#2513,.T.);
#5018=EDGE_CURVE('',#4127,#4127,#3566,.T.);
#5019=EDGE_CURVE('',#4128,#4128,#3567,.T.);
#5020=EDGE_CURVE('',#4128,#4129,#2514,.T.);
#5021=EDGE_CURVE('',#4129,#4129,#3568,.T.);
#5022=EDGE_CURVE('',#4130,#4130,#3569,.T.);
#5023=EDGE_CURVE('',#4130,#4131,#2515,.T.);
#5024=EDGE_CURVE('',#4131,#4131,#3570,.T.);
#5025=EDGE_CURVE('',#4132,#4132,#3571,.T.);
#5026=EDGE_CURVE('',#4132,#4133,#2516,.T.);
#5027=EDGE_CURVE('',#4133,#4133,#3572,.T.);
#5028=EDGE_CURVE('',#4134,#4134,#3573,.T.);
#5029=EDGE_CURVE('',#4134,#4135,#2517,.T.);
#5030=EDGE_CURVE('',#4135,#4135,#3574,.T.);
#5031=EDGE_CURVE('',#4136,#4136,#3575,.T.);
#5032=EDGE_CURVE('',#4136,#4137,#2518,.T.);
#5033=EDGE_CURVE('',#4137,#4137,#3576,.T.);
#5034=EDGE_CURVE('',#4138,#4138,#3577,.T.);
#5035=EDGE_CURVE('',#4138,#4139,#2519,.T.);
#5036=EDGE_CURVE('',#4139,#4139,#3578,.T.);
#5037=EDGE_CURVE('',#4140,#4140,#3579,.T.);
#5038=EDGE_CURVE('',#4140,#4141,#2520,.T.);
#5039=EDGE_CURVE('',#4141,#4141,#3580,.T.);
#5040=EDGE_CURVE('',#4142,#4143,#2521,.T.);
#5041=EDGE_CURVE('',#4143,#4144,#2522,.T.);
#5042=EDGE_CURVE('',#4145,#4144,#2523,.T.);
#5043=EDGE_CURVE('',#4142,#4145,#2524,.T.);
#5044=EDGE_CURVE('',#4146,#4142,#2525,.T.);
#5045=EDGE_CURVE('',#4147,#4145,#2526,.T.);
#5046=EDGE_CURVE('',#4146,#4147,#2527,.T.);
#5047=EDGE_CURVE('',#4148,#4146,#2528,.T.);
#5048=EDGE_CURVE('',#4149,#4147,#2529,.T.);
#5049=EDGE_CURVE('',#4148,#4149,#2530,.T.);
#5050=EDGE_CURVE('',#4143,#4148,#2531,.T.);
#5051=EDGE_CURVE('',#4144,#4149,#2532,.T.);
#5052=EDGE_CURVE('',#4150,#4150,#3581,.T.);
#5053=EDGE_CURVE('',#4150,#4151,#2533,.T.);
#5054=EDGE_CURVE('',#4151,#4151,#3582,.T.);
#5055=EDGE_CURVE('',#4152,#4152,#3583,.T.);
#5056=EDGE_CURVE('',#4153,#4153,#3584,.T.);
#5057=EDGE_CURVE('',#4154,#4154,#3585,.T.);
#5058=EDGE_CURVE('',#4155,#4155,#3586,.T.);
#5059=EDGE_CURVE('',#4152,#4154,#2534,.T.);
#5060=EDGE_CURVE('',#4155,#4156,#2535,.T.);
#5061=EDGE_CURVE('',#4156,#4156,#3587,.T.);
#5062=EDGE_CURVE('',#4157,#4157,#3588,.T.);
#5063=EDGE_CURVE('',#4157,#4153,#2536,.T.);
#5064=EDGE_CURVE('',#4158,#4158,#3589,.T.);
#5065=EDGE_CURVE('',#4158,#4159,#2537,.T.);
#5066=EDGE_CURVE('',#4159,#4159,#3590,.T.);
#5067=EDGE_CURVE('',#4160,#4160,#3591,.T.);
#5068=EDGE_CURVE('',#4160,#4161,#2538,.T.);
#5069=EDGE_CURVE('',#4161,#4161,#3592,.T.);
#5070=EDGE_CURVE('',#4162,#4162,#3593,.T.);
#5071=EDGE_CURVE('',#4162,#4163,#2539,.T.);
#5072=EDGE_CURVE('',#4163,#4163,#3594,.T.);
#5073=EDGE_CURVE('',#4164,#4164,#3595,.T.);
#5074=EDGE_CURVE('',#4164,#4165,#2540,.T.);
#5075=EDGE_CURVE('',#4165,#4165,#3596,.T.);
#5076=EDGE_CURVE('',#4166,#4166,#3597,.T.);
#5077=EDGE_CURVE('',#4166,#4167,#2541,.T.);
#5078=EDGE_CURVE('',#4167,#4167,#3598,.T.);
#5079=EDGE_CURVE('',#4168,#4168,#3599,.T.);
#5080=EDGE_CURVE('',#4168,#4169,#2542,.T.);
#5081=EDGE_CURVE('',#4169,#4169,#3600,.T.);
#5082=EDGE_CURVE('',#4170,#4171,#2543,.T.);
#5083=EDGE_CURVE('',#4170,#4171,#3601,.T.);
#5084=EDGE_CURVE('',#4172,#4170,#2544,.T.);
#5085=EDGE_CURVE('',#4173,#4172,#3602,.T.);
#5086=EDGE_CURVE('',#4173,#4174,#2545,.T.);
#5087=EDGE_CURVE('',#4174,#4174,#3603,.T.);
#5088=EDGE_CURVE('',#4175,#4173,#3604,.T.);
#5089=EDGE_CURVE('',#4171,#4175,#2546,.T.);
#5090=EDGE_CURVE('',#4176,#4177,#2547,.T.);
#5091=EDGE_CURVE('',#4176,#4177,#3605,.T.);
#5092=EDGE_CURVE('',#4178,#4176,#2548,.T.);
#5093=EDGE_CURVE('',#4179,#4178,#3606,.T.);
#5094=EDGE_CURVE('',#4179,#4180,#2549,.T.);
#5095=EDGE_CURVE('',#4180,#4180,#3607,.T.);
#5096=EDGE_CURVE('',#4181,#4179,#3608,.T.);
#5097=EDGE_CURVE('',#4177,#4181,#2550,.T.);
#5098=EDGE_CURVE('',#4182,#4183,#2551,.T.);
#5099=EDGE_CURVE('',#4182,#4183,#3609,.T.);
#5100=EDGE_CURVE('',#4184,#4182,#2552,.T.);
#5101=EDGE_CURVE('',#4185,#4184,#3610,.T.);
#5102=EDGE_CURVE('',#4185,#4186,#2553,.T.);
#5103=EDGE_CURVE('',#4186,#4186,#3611,.T.);
#5104=EDGE_CURVE('',#4187,#4185,#3612,.T.);
#5105=EDGE_CURVE('',#4183,#4187,#2554,.T.);
#5106=EDGE_CURVE('',#4188,#4189,#2555,.T.);
#5107=EDGE_CURVE('',#4188,#4189,#3613,.T.);
#5108=EDGE_CURVE('',#4190,#4188,#2556,.T.);
#5109=EDGE_CURVE('',#4191,#4190,#3614,.T.);
#5110=EDGE_CURVE('',#4191,#4192,#2557,.T.);
#5111=EDGE_CURVE('',#4192,#4192,#3615,.T.);
#5112=EDGE_CURVE('',#4193,#4191,#3616,.T.);
#5113=EDGE_CURVE('',#4189,#4193,#2558,.T.);
#5114=EDGE_CURVE('',#4175,#4184,#2559,.T.);
#5115=EDGE_CURVE('',#4187,#4194,#2560,.T.);
#5116=EDGE_CURVE('',#4195,#4194,#2561,.T.);
#5117=EDGE_CURVE('',#4195,#4196,#2562,.T.);
#5118=EDGE_CURVE('',#4197,#4196,#2563,.T.);
#5119=EDGE_CURVE('',#4197,#4172,#2564,.T.);
#5120=EDGE_CURVE('',#4181,#4190,#2565,.T.);
#5121=EDGE_CURVE('',#4193,#4198,#2566,.T.);
#5122=EDGE_CURVE('',#4199,#4198,#2567,.T.);
#5123=EDGE_CURVE('',#4200,#4199,#2568,.T.);
#5124=EDGE_CURVE('',#4201,#4200,#2569,.T.);
#5125=EDGE_CURVE('',#4201,#4178,#2570,.T.);
#5126=EDGE_CURVE('',#4194,#4202,#2571,.T.);
#5127=EDGE_CURVE('',#4202,#4203,#2572,.T.);
#5128=EDGE_CURVE('',#4203,#4204,#2573,.T.);
#5129=EDGE_CURVE('',#4204,#4205,#2574,.T.);
#5130=EDGE_CURVE('',#4205,#4201,#2575,.T.);
#5131=EDGE_CURVE('',#4200,#4206,#2576,.T.);
#5132=EDGE_CURVE('',#4206,#4207,#2577,.T.);
#5133=EDGE_CURVE('',#4207,#4208,#2578,.T.);
#5134=EDGE_CURVE('',#4208,#4209,#2579,.T.);
#5135=EDGE_CURVE('',#4209,#4195,#2580,.T.);
#5136=EDGE_CURVE('',#4210,#4197,#2581,.T.);
#5137=EDGE_CURVE('',#4202,#4210,#2582,.T.);
#5138=EDGE_CURVE('',#4211,#4210,#2583,.T.);
#5139=EDGE_CURVE('',#4203,#4211,#2584,.T.);
#5140=EDGE_CURVE('',#4212,#4211,#2585,.T.);
#5141=EDGE_CURVE('',#4204,#4212,#2586,.T.);
#5142=EDGE_CURVE('',#4213,#4212,#2587,.T.);
#5143=EDGE_CURVE('',#4205,#4213,#2588,.T.);
#5144=EDGE_CURVE('',#4198,#4213,#2589,.T.);
#5145=EDGE_CURVE('',#4214,#4199,#2590,.T.);
#5146=EDGE_CURVE('',#4206,#4214,#2591,.T.);
#5147=EDGE_CURVE('',#4215,#4214,#2592,.T.);
#5148=EDGE_CURVE('',#4207,#4215,#2593,.T.);
#5149=EDGE_CURVE('',#4216,#4215,#2594,.T.);
#5150=EDGE_CURVE('',#4208,#4216,#2595,.T.);
#5151=EDGE_CURVE('',#4217,#4216,#2596,.T.);
#5152=EDGE_CURVE('',#4209,#4217,#2597,.T.);
#5153=EDGE_CURVE('',#4196,#4217,#2598,.T.);
#5154=EDGE_CURVE('',#4218,#4219,#2599,.T.);
#5155=EDGE_CURVE('',#4219,#4220,#2600,.T.);
#5156=EDGE_CURVE('',#4221,#4220,#2601,.T.);
#5157=EDGE_CURVE('',#4218,#4221,#2602,.T.);
#5158=EDGE_CURVE('',#4222,#4218,#2603,.T.);
#5159=EDGE_CURVE('',#4223,#4221,#2604,.T.);
#5160=EDGE_CURVE('',#4222,#4223,#2605,.T.);
#5161=EDGE_CURVE('',#4224,#4222,#2606,.T.);
#5162=EDGE_CURVE('',#4225,#4223,#2607,.T.);
#5163=EDGE_CURVE('',#4224,#4225,#2608,.T.);
#5164=EDGE_CURVE('',#4226,#4224,#2609,.T.);
#5165=EDGE_CURVE('',#4227,#4225,#2610,.T.);
#5166=EDGE_CURVE('',#4226,#4227,#2611,.T.);
#5167=EDGE_CURVE('',#4228,#4226,#2612,.T.);
#5168=EDGE_CURVE('',#4229,#4227,#2613,.T.);
#5169=EDGE_CURVE('',#4228,#4229,#2614,.T.);
#5170=EDGE_CURVE('',#4230,#4228,#2615,.T.);
#5171=EDGE_CURVE('',#4231,#4229,#2616,.T.);
#5172=EDGE_CURVE('',#4230,#4231,#2617,.T.);
#5173=EDGE_CURVE('',#4232,#4230,#2618,.T.);
#5174=EDGE_CURVE('',#4233,#4231,#2619,.T.);
#5175=EDGE_CURVE('',#4232,#4233,#2620,.T.);
#5176=EDGE_CURVE('',#4219,#4232,#2621,.T.);
#5177=EDGE_CURVE('',#4220,#4233,#2622,.T.);
#5178=EDGE_CURVE('',#4234,#4235,#2623,.T.);
#5179=EDGE_CURVE('',#4234,#4236,#2624,.T.);
#5180=EDGE_CURVE('',#4237,#4236,#2625,.T.);
#5181=EDGE_CURVE('',#4235,#4237,#2626,.T.);
#5182=EDGE_CURVE('',#4235,#4238,#2627,.T.);
#5183=EDGE_CURVE('',#4239,#4237,#2628,.T.);
#5184=EDGE_CURVE('',#4238,#4239,#2629,.T.);
#5185=EDGE_CURVE('',#4238,#4240,#2630,.T.);
#5186=EDGE_CURVE('',#4241,#4239,#2631,.T.);
#5187=EDGE_CURVE('',#4240,#4241,#2632,.T.);
#5188=EDGE_CURVE('',#4240,#4242,#2633,.T.);
#5189=EDGE_CURVE('',#4243,#4241,#2634,.T.);
#5190=EDGE_CURVE('',#4242,#4243,#2635,.T.);
#5191=EDGE_CURVE('',#4242,#4244,#2636,.T.);
#5192=EDGE_CURVE('',#4245,#4243,#2637,.T.);
#5193=EDGE_CURVE('',#4244,#4245,#2638,.T.);
#5194=EDGE_CURVE('',#4244,#4246,#2639,.T.);
#5195=EDGE_CURVE('',#4247,#4245,#2640,.T.);
#5196=EDGE_CURVE('',#4246,#4247,#2641,.T.);
#5197=EDGE_CURVE('',#4246,#4248,#2642,.T.);
#5198=EDGE_CURVE('',#4249,#4247,#2643,.T.);
#5199=EDGE_CURVE('',#4248,#4249,#2644,.T.);
#5200=EDGE_CURVE('',#4248,#4234,#2645,.T.);
#5201=EDGE_CURVE('',#4236,#4249,#2646,.T.);
#5202=EDGE_CURVE('',#4250,#4251,#2647,.T.);
#5203=EDGE_CURVE('',#4251,#4252,#2648,.T.);
#5204=EDGE_CURVE('',#4252,#4253,#2649,.T.);
#5205=EDGE_CURVE('',#4250,#4253,#2650,.T.);
#5206=EDGE_CURVE('',#4251,#4254,#2651,.T.);
#5207=EDGE_CURVE('',#4254,#4255,#2652,.T.);
#5208=EDGE_CURVE('',#4255,#4252,#2653,.T.);
#5209=EDGE_CURVE('',#4254,#4256,#2654,.T.);
#5210=EDGE_CURVE('',#4256,#4257,#2655,.T.);
#5211=EDGE_CURVE('',#4257,#4255,#2656,.T.);
#5212=EDGE_CURVE('',#4256,#4258,#2657,.T.);
#5213=EDGE_CURVE('',#4258,#4259,#2658,.T.);
#5214=EDGE_CURVE('',#4259,#4257,#2659,.T.);
#5215=EDGE_CURVE('',#4258,#4260,#2660,.T.);
#5216=EDGE_CURVE('',#4260,#4261,#2661,.T.);
#5217=EDGE_CURVE('',#4261,#4259,#2662,.T.);
#5218=EDGE_CURVE('',#4260,#4250,#2663,.T.);
#5219=EDGE_CURVE('',#4253,#4261,#2664,.T.);
#5220=EDGE_CURVE('',#4262,#4262,#3617,.T.);
#5221=EDGE_CURVE('',#4263,#4263,#3618,.T.);
#5222=EDGE_CURVE('',#4264,#4264,#3619,.T.);
#5223=EDGE_CURVE('',#4264,#4263,#2665,.T.);
#5224=EDGE_CURVE('',#4265,#4265,#3620,.T.);
#5225=EDGE_CURVE('',#4265,#4264,#2666,.T.);
#5226=EDGE_CURVE('',#4266,#4266,#3621,.T.);
#5227=EDGE_CURVE('',#4266,#4265,#2667,.T.);
#5228=EDGE_CURVE('',#4267,#4267,#3622,.T.);
#5229=EDGE_CURVE('',#4268,#4268,#3623,.F.);
#5230=EDGE_CURVE('',#4268,#4267,#2668,.T.);
#5231=EDGE_CURVE('',#4262,#4268,#2669,.T.);
#5232=EDGE_CURVE('',#4269,#4270,#2670,.T.);
#5233=EDGE_CURVE('',#4270,#4271,#2671,.T.);
#5234=EDGE_CURVE('',#4271,#4272,#2672,.T.);
#5235=EDGE_CURVE('',#4269,#4272,#2673,.T.);
#5236=EDGE_CURVE('',#4270,#4273,#2674,.T.);
#5237=EDGE_CURVE('',#4273,#4274,#2675,.T.);
#5238=EDGE_CURVE('',#4274,#4271,#2676,.T.);
#5239=EDGE_CURVE('',#4273,#4275,#2677,.T.);
#5240=EDGE_CURVE('',#4275,#4276,#2678,.T.);
#5241=EDGE_CURVE('',#4276,#4274,#2679,.T.);
#5242=EDGE_CURVE('',#4275,#4277,#2680,.T.);
#5243=EDGE_CURVE('',#4277,#4278,#2681,.T.);
#5244=EDGE_CURVE('',#4278,#4276,#2682,.T.);
#5245=EDGE_CURVE('',#4277,#4279,#2683,.T.);
#5246=EDGE_CURVE('',#4279,#4280,#2684,.T.);
#5247=EDGE_CURVE('',#4280,#4278,#2685,.T.);
#5248=EDGE_CURVE('',#4279,#4269,#2686,.T.);
#5249=EDGE_CURVE('',#4272,#4280,#2687,.T.);
#5250=EDGE_CURVE('',#4281,#4281,#3624,.T.);
#5251=EDGE_CURVE('',#4282,#4282,#3625,.T.);
#5252=EDGE_CURVE('',#4283,#4283,#3626,.T.);
#5253=EDGE_CURVE('',#4283,#4282,#2688,.T.);
#5254=EDGE_CURVE('',#4284,#4284,#3627,.T.);
#5255=EDGE_CURVE('',#4284,#4283,#2689,.T.);
#5256=EDGE_CURVE('',#4285,#4285,#3628,.T.);
#5257=EDGE_CURVE('',#4285,#4284,#2690,.T.);
#5258=EDGE_CURVE('',#4286,#4286,#3629,.T.);
#5259=EDGE_CURVE('',#4287,#4287,#3630,.F.);
#5260=EDGE_CURVE('',#4287,#4286,#2691,.T.);
#5261=EDGE_CURVE('',#4281,#4287,#2692,.T.);
#5262=ORIENTED_EDGE('',*,*,#4288,.F.);
#5263=ORIENTED_EDGE('',*,*,#4289,.T.);
#5264=ORIENTED_EDGE('',*,*,#4290,.F.);
#5265=ORIENTED_EDGE('',*,*,#4289,.F.);
#5266=ORIENTED_EDGE('',*,*,#4291,.F.);
#5267=ORIENTED_EDGE('',*,*,#4292,.T.);
#5268=ORIENTED_EDGE('',*,*,#4293,.F.);
#5269=ORIENTED_EDGE('',*,*,#4292,.F.);
#5270=ORIENTED_EDGE('',*,*,#4294,.F.);
#5271=ORIENTED_EDGE('',*,*,#4295,.T.);
#5272=ORIENTED_EDGE('',*,*,#4296,.F.);
#5273=ORIENTED_EDGE('',*,*,#4295,.F.);
#5274=ORIENTED_EDGE('',*,*,#4297,.F.);
#5275=ORIENTED_EDGE('',*,*,#4298,.T.);
#5276=ORIENTED_EDGE('',*,*,#4299,.F.);
#5277=ORIENTED_EDGE('',*,*,#4298,.F.);
#5278=ORIENTED_EDGE('',*,*,#4300,.F.);
#5279=ORIENTED_EDGE('',*,*,#4301,.T.);
#5280=ORIENTED_EDGE('',*,*,#4302,.F.);
#5281=ORIENTED_EDGE('',*,*,#4301,.F.);
#5282=ORIENTED_EDGE('',*,*,#4303,.F.);
#5283=ORIENTED_EDGE('',*,*,#4304,.T.);
#5284=ORIENTED_EDGE('',*,*,#4305,.F.);
#5285=ORIENTED_EDGE('',*,*,#4304,.F.);
#5286=ORIENTED_EDGE('',*,*,#4306,.F.);
#5287=ORIENTED_EDGE('',*,*,#4307,.T.);
#5288=ORIENTED_EDGE('',*,*,#4308,.F.);
#5289=ORIENTED_EDGE('',*,*,#4307,.F.);
#5290=ORIENTED_EDGE('',*,*,#4309,.F.);
#5291=ORIENTED_EDGE('',*,*,#4310,.T.);
#5292=ORIENTED_EDGE('',*,*,#4311,.F.);
#5293=ORIENTED_EDGE('',*,*,#4310,.F.);
#5294=ORIENTED_EDGE('',*,*,#4312,.F.);
#5295=ORIENTED_EDGE('',*,*,#4313,.T.);
#5296=ORIENTED_EDGE('',*,*,#4314,.F.);
#5297=ORIENTED_EDGE('',*,*,#4313,.F.);
#5298=ORIENTED_EDGE('',*,*,#4315,.F.);
#5299=ORIENTED_EDGE('',*,*,#4316,.T.);
#5300=ORIENTED_EDGE('',*,*,#4317,.F.);
#5301=ORIENTED_EDGE('',*,*,#4316,.F.);
#5302=ORIENTED_EDGE('',*,*,#4318,.F.);
#5303=ORIENTED_EDGE('',*,*,#4319,.T.);
#5304=ORIENTED_EDGE('',*,*,#4320,.F.);
#5305=ORIENTED_EDGE('',*,*,#4319,.F.);
#5306=ORIENTED_EDGE('',*,*,#4321,.F.);
#5307=ORIENTED_EDGE('',*,*,#4322,.T.);
#5308=ORIENTED_EDGE('',*,*,#4323,.F.);
#5309=ORIENTED_EDGE('',*,*,#4322,.F.);
#5310=ORIENTED_EDGE('',*,*,#4324,.T.);
#5311=ORIENTED_EDGE('',*,*,#4325,.T.);
#5312=ORIENTED_EDGE('',*,*,#4326,.F.);
#5313=ORIENTED_EDGE('',*,*,#4327,.F.);
#5314=ORIENTED_EDGE('',*,*,#4328,.T.);
#5315=ORIENTED_EDGE('',*,*,#4327,.T.);
#5316=ORIENTED_EDGE('',*,*,#4329,.F.);
#5317=ORIENTED_EDGE('',*,*,#4330,.F.);
#5318=ORIENTED_EDGE('',*,*,#4331,.T.);
#5319=ORIENTED_EDGE('',*,*,#4330,.T.);
#5320=ORIENTED_EDGE('',*,*,#4332,.F.);
#5321=ORIENTED_EDGE('',*,*,#4333,.F.);
#5322=ORIENTED_EDGE('',*,*,#4334,.T.);
#5323=ORIENTED_EDGE('',*,*,#4333,.T.);
#5324=ORIENTED_EDGE('',*,*,#4335,.F.);
#5325=ORIENTED_EDGE('',*,*,#4325,.F.);
#5326=ORIENTED_EDGE('',*,*,#4335,.T.);
#5327=ORIENTED_EDGE('',*,*,#4332,.T.);
#5328=ORIENTED_EDGE('',*,*,#4329,.T.);
#5329=ORIENTED_EDGE('',*,*,#4326,.T.);
#5330=ORIENTED_EDGE('',*,*,#4302,.T.);
#5331=ORIENTED_EDGE('',*,*,#4305,.T.);
#5332=ORIENTED_EDGE('',*,*,#4308,.T.);
#5333=ORIENTED_EDGE('',*,*,#4311,.T.);
#5334=ORIENTED_EDGE('',*,*,#4314,.T.);
#5335=ORIENTED_EDGE('',*,*,#4317,.T.);
#5336=ORIENTED_EDGE('',*,*,#4320,.T.);
#5337=ORIENTED_EDGE('',*,*,#4323,.T.);
#5338=ORIENTED_EDGE('',*,*,#4299,.T.);
#5339=ORIENTED_EDGE('',*,*,#4296,.T.);
#5340=ORIENTED_EDGE('',*,*,#4293,.T.);
#5341=ORIENTED_EDGE('',*,*,#4290,.T.);
#5342=ORIENTED_EDGE('',*,*,#4334,.F.);
#5343=ORIENTED_EDGE('',*,*,#4324,.F.);
#5344=ORIENTED_EDGE('',*,*,#4328,.F.);
#5345=ORIENTED_EDGE('',*,*,#4331,.F.);
#5346=ORIENTED_EDGE('',*,*,#4300,.T.);
#5347=ORIENTED_EDGE('',*,*,#4303,.T.);
#5348=ORIENTED_EDGE('',*,*,#4306,.T.);
#5349=ORIENTED_EDGE('',*,*,#4309,.T.);
#5350=ORIENTED_EDGE('',*,*,#4312,.T.);
#5351=ORIENTED_EDGE('',*,*,#4315,.T.);
#5352=ORIENTED_EDGE('',*,*,#4318,.T.);
#5353=ORIENTED_EDGE('',*,*,#4321,.T.);
#5354=ORIENTED_EDGE('',*,*,#4297,.T.);
#5355=ORIENTED_EDGE('',*,*,#4294,.T.);
#5356=ORIENTED_EDGE('',*,*,#4291,.T.);
#5357=ORIENTED_EDGE('',*,*,#4288,.T.);
#5358=ORIENTED_EDGE('',*,*,#4336,.T.);
#5359=ORIENTED_EDGE('',*,*,#4337,.T.);
#5360=ORIENTED_EDGE('',*,*,#4338,.F.);
#5361=ORIENTED_EDGE('',*,*,#4339,.F.);
#5362=ORIENTED_EDGE('',*,*,#4340,.T.);
#5363=ORIENTED_EDGE('',*,*,#4339,.T.);
#5364=ORIENTED_EDGE('',*,*,#4341,.F.);
#5365=ORIENTED_EDGE('',*,*,#4342,.F.);
#5366=ORIENTED_EDGE('',*,*,#4343,.T.);
#5367=ORIENTED_EDGE('',*,*,#4342,.T.);
#5368=ORIENTED_EDGE('',*,*,#4344,.F.);
#5369=ORIENTED_EDGE('',*,*,#4345,.F.);
#5370=ORIENTED_EDGE('',*,*,#4346,.T.);
#5371=ORIENTED_EDGE('',*,*,#4345,.T.);
#5372=ORIENTED_EDGE('',*,*,#4347,.F.);
#5373=ORIENTED_EDGE('',*,*,#4337,.F.);
#5374=ORIENTED_EDGE('',*,*,#4347,.T.);
#5375=ORIENTED_EDGE('',*,*,#4344,.T.);
#5376=ORIENTED_EDGE('',*,*,#4341,.T.);
#5377=ORIENTED_EDGE('',*,*,#4338,.T.);
#5378=ORIENTED_EDGE('',*,*,#4346,.F.);
#5379=ORIENTED_EDGE('',*,*,#4336,.F.);
#5380=ORIENTED_EDGE('',*,*,#4340,.F.);
#5381=ORIENTED_EDGE('',*,*,#4343,.F.);
#5382=ORIENTED_EDGE('',*,*,#4348,.T.);
#5383=ORIENTED_EDGE('',*,*,#4349,.T.);
#5384=ORIENTED_EDGE('',*,*,#4350,.F.);
#5385=ORIENTED_EDGE('',*,*,#4351,.F.);
#5386=ORIENTED_EDGE('',*,*,#4352,.T.);
#5387=ORIENTED_EDGE('',*,*,#4351,.T.);
#5388=ORIENTED_EDGE('',*,*,#4353,.F.);
#5389=ORIENTED_EDGE('',*,*,#4354,.F.);
#5390=ORIENTED_EDGE('',*,*,#4355,.T.);
#5391=ORIENTED_EDGE('',*,*,#4354,.T.);
#5392=ORIENTED_EDGE('',*,*,#4356,.F.);
#5393=ORIENTED_EDGE('',*,*,#4357,.F.);
#5394=ORIENTED_EDGE('',*,*,#4358,.T.);
#5395=ORIENTED_EDGE('',*,*,#4357,.T.);
#5396=ORIENTED_EDGE('',*,*,#4359,.F.);
#5397=ORIENTED_EDGE('',*,*,#4349,.F.);
#5398=ORIENTED_EDGE('',*,*,#4359,.T.);
#5399=ORIENTED_EDGE('',*,*,#4356,.T.);
#5400=ORIENTED_EDGE('',*,*,#4353,.T.);
#5401=ORIENTED_EDGE('',*,*,#4350,.T.);
#5402=ORIENTED_EDGE('',*,*,#4358,.F.);
#5403=ORIENTED_EDGE('',*,*,#4348,.F.);
#5404=ORIENTED_EDGE('',*,*,#4352,.F.);
#5405=ORIENTED_EDGE('',*,*,#4355,.F.);
#5406=ORIENTED_EDGE('',*,*,#4360,.F.);
#5407=ORIENTED_EDGE('',*,*,#4361,.F.);
#5408=ORIENTED_EDGE('',*,*,#4362,.T.);
#5409=ORIENTED_EDGE('',*,*,#4363,.F.);
#5410=ORIENTED_EDGE('',*,*,#4364,.F.);
#5411=ORIENTED_EDGE('',*,*,#4362,.F.);
#5412=ORIENTED_EDGE('',*,*,#4365,.F.);
#5413=ORIENTED_EDGE('',*,*,#4366,.T.);
#5414=ORIENTED_EDGE('',*,*,#4367,.F.);
#5415=ORIENTED_EDGE('',*,*,#4366,.F.);
#5416=ORIENTED_EDGE('',*,*,#4365,.T.);
#5417=ORIENTED_EDGE('',*,*,#4368,.F.);
#5418=ORIENTED_EDGE('',*,*,#4369,.T.);
#5419=ORIENTED_EDGE('',*,*,#4370,.F.);
#5420=ORIENTED_EDGE('',*,*,#4369,.F.);
#5421=ORIENTED_EDGE('',*,*,#4368,.T.);
#5422=ORIENTED_EDGE('',*,*,#4371,.F.);
#5423=ORIENTED_EDGE('',*,*,#4372,.T.);
#5424=ORIENTED_EDGE('',*,*,#4373,.F.);
#5425=ORIENTED_EDGE('',*,*,#4372,.F.);
#5426=ORIENTED_EDGE('',*,*,#4371,.T.);
#5427=ORIENTED_EDGE('',*,*,#4374,.F.);
#5428=ORIENTED_EDGE('',*,*,#4375,.T.);
#5429=ORIENTED_EDGE('',*,*,#4376,.F.);
#5430=ORIENTED_EDGE('',*,*,#4375,.F.);
#5431=ORIENTED_EDGE('',*,*,#4374,.T.);
#5432=ORIENTED_EDGE('',*,*,#4377,.F.);
#5433=ORIENTED_EDGE('',*,*,#4378,.T.);
#5434=ORIENTED_EDGE('',*,*,#4379,.F.);
#5435=ORIENTED_EDGE('',*,*,#4380,.F.);
#5436=ORIENTED_EDGE('',*,*,#4381,.F.);
#5437=ORIENTED_EDGE('',*,*,#4378,.F.);
#5438=ORIENTED_EDGE('',*,*,#4382,.F.);
#5439=ORIENTED_EDGE('',*,*,#4383,.T.);
#5440=ORIENTED_EDGE('',*,*,#4384,.F.);
#5441=ORIENTED_EDGE('',*,*,#4385,.F.);
#5442=ORIENTED_EDGE('',*,*,#4386,.F.);
#5443=ORIENTED_EDGE('',*,*,#4383,.F.);
#5444=ORIENTED_EDGE('',*,*,#4387,.F.);
#5445=ORIENTED_EDGE('',*,*,#4388,.T.);
#5446=ORIENTED_EDGE('',*,*,#4389,.F.);
#5447=ORIENTED_EDGE('',*,*,#4390,.F.);
#5448=ORIENTED_EDGE('',*,*,#4391,.F.);
#5449=ORIENTED_EDGE('',*,*,#4388,.F.);
#5450=ORIENTED_EDGE('',*,*,#4392,.F.);
#5451=ORIENTED_EDGE('',*,*,#4393,.T.);
#5452=ORIENTED_EDGE('',*,*,#4394,.F.);
#5453=ORIENTED_EDGE('',*,*,#4395,.F.);
#5454=ORIENTED_EDGE('',*,*,#4396,.F.);
#5455=ORIENTED_EDGE('',*,*,#4393,.F.);
#5456=ORIENTED_EDGE('',*,*,#4397,.T.);
#5457=ORIENTED_EDGE('',*,*,#4398,.F.);
#5458=ORIENTED_EDGE('',*,*,#4385,.T.);
#5459=ORIENTED_EDGE('',*,*,#4399,.F.);
#5460=ORIENTED_EDGE('',*,*,#4390,.T.);
#5461=ORIENTED_EDGE('',*,*,#4400,.F.);
#5462=ORIENTED_EDGE('',*,*,#4395,.T.);
#5463=ORIENTED_EDGE('',*,*,#4401,.F.);
#5464=ORIENTED_EDGE('',*,*,#4380,.T.);
#5465=ORIENTED_EDGE('',*,*,#4402,.F.);
#5466=ORIENTED_EDGE('',*,*,#4403,.T.);
#5467=ORIENTED_EDGE('',*,*,#4404,.T.);
#5468=ORIENTED_EDGE('',*,*,#4405,.T.);
#5469=ORIENTED_EDGE('',*,*,#4406,.T.);
#5470=ORIENTED_EDGE('',*,*,#4407,.F.);
#5471=ORIENTED_EDGE('',*,*,#4408,.T.);
#5472=ORIENTED_EDGE('',*,*,#4403,.F.);
#5473=ORIENTED_EDGE('',*,*,#4408,.F.);
#5474=ORIENTED_EDGE('',*,*,#4409,.F.);
#5475=ORIENTED_EDGE('',*,*,#4410,.T.);
#5476=ORIENTED_EDGE('',*,*,#4404,.F.);
#5477=ORIENTED_EDGE('',*,*,#4410,.F.);
#5478=ORIENTED_EDGE('',*,*,#4411,.F.);
#5479=ORIENTED_EDGE('',*,*,#4412,.T.);
#5480=ORIENTED_EDGE('',*,*,#4405,.F.);
#5481=ORIENTED_EDGE('',*,*,#4412,.F.);
#5482=ORIENTED_EDGE('',*,*,#4413,.F.);
#5483=ORIENTED_EDGE('',*,*,#4414,.T.);
#5484=ORIENTED_EDGE('',*,*,#4406,.F.);
#5485=ORIENTED_EDGE('',*,*,#4414,.F.);
#5486=ORIENTED_EDGE('',*,*,#4415,.F.);
#5487=ORIENTED_EDGE('',*,*,#4416,.T.);
#5488=ORIENTED_EDGE('',*,*,#4402,.T.);
#5489=ORIENTED_EDGE('',*,*,#4379,.T.);
#5490=ORIENTED_EDGE('',*,*,#4381,.T.);
#5491=ORIENTED_EDGE('',*,*,#4377,.T.);
#5492=ORIENTED_EDGE('',*,*,#4401,.T.);
#5493=ORIENTED_EDGE('',*,*,#4394,.T.);
#5494=ORIENTED_EDGE('',*,*,#4396,.T.);
#5495=ORIENTED_EDGE('',*,*,#4392,.T.);
#5496=ORIENTED_EDGE('',*,*,#4400,.T.);
#5497=ORIENTED_EDGE('',*,*,#4389,.T.);
#5498=ORIENTED_EDGE('',*,*,#4391,.T.);
#5499=ORIENTED_EDGE('',*,*,#4387,.T.);
#5500=ORIENTED_EDGE('',*,*,#4399,.T.);
#5501=ORIENTED_EDGE('',*,*,#4384,.T.);
#5502=ORIENTED_EDGE('',*,*,#4386,.T.);
#5503=ORIENTED_EDGE('',*,*,#4382,.T.);
#5504=ORIENTED_EDGE('',*,*,#4398,.T.);
#5505=ORIENTED_EDGE('',*,*,#4416,.F.);
#5506=ORIENTED_EDGE('',*,*,#4417,.F.);
#5507=ORIENTED_EDGE('',*,*,#4418,.T.);
#5508=ORIENTED_EDGE('',*,*,#4419,.F.);
#5509=ORIENTED_EDGE('',*,*,#4418,.F.);
#5510=ORIENTED_EDGE('',*,*,#4417,.T.);
#5511=ORIENTED_EDGE('',*,*,#4420,.F.);
#5512=ORIENTED_EDGE('',*,*,#4397,.F.);
#5513=ORIENTED_EDGE('',*,*,#4421,.T.);
#5514=ORIENTED_EDGE('',*,*,#4422,.T.);
#5515=ORIENTED_EDGE('',*,*,#4421,.F.);
#5516=ORIENTED_EDGE('',*,*,#4363,.T.);
#5517=ORIENTED_EDGE('',*,*,#4364,.T.);
#5518=ORIENTED_EDGE('',*,*,#4420,.T.);
#5519=ORIENTED_EDGE('',*,*,#4423,.T.);
#5520=ORIENTED_EDGE('',*,*,#4424,.T.);
#5521=ORIENTED_EDGE('',*,*,#4423,.F.);
#5522=ORIENTED_EDGE('',*,*,#4360,.T.);
#5523=ORIENTED_EDGE('',*,*,#4361,.T.);
#5524=ORIENTED_EDGE('',*,*,#4415,.T.);
#5525=ORIENTED_EDGE('',*,*,#4419,.T.);
#5526=ORIENTED_EDGE('',*,*,#4376,.T.);
#5527=ORIENTED_EDGE('',*,*,#4373,.T.);
#5528=ORIENTED_EDGE('',*,*,#4370,.T.);
#5529=ORIENTED_EDGE('',*,*,#4367,.T.);
#5530=ORIENTED_EDGE('',*,*,#4422,.F.);
#5531=ORIENTED_EDGE('',*,*,#4424,.F.);
#5532=ORIENTED_EDGE('',*,*,#4413,.T.);
#5533=ORIENTED_EDGE('',*,*,#4411,.T.);
#5534=ORIENTED_EDGE('',*,*,#4409,.T.);
#5535=ORIENTED_EDGE('',*,*,#4407,.T.);
#5536=ORIENTED_EDGE('',*,*,#4425,.F.);
#5537=ORIENTED_EDGE('',*,*,#4426,.T.);
#5538=ORIENTED_EDGE('',*,*,#4427,.F.);
#5539=ORIENTED_EDGE('',*,*,#4426,.F.);
#5540=ORIENTED_EDGE('',*,*,#4425,.T.);
#5541=ORIENTED_EDGE('',*,*,#4428,.F.);
#5542=ORIENTED_EDGE('',*,*,#4429,.F.);
#5543=ORIENTED_EDGE('',*,*,#4430,.T.);
#5544=ORIENTED_EDGE('',*,*,#4431,.F.);
#5545=ORIENTED_EDGE('',*,*,#4430,.F.);
#5546=ORIENTED_EDGE('',*,*,#4429,.T.);
#5547=ORIENTED_EDGE('',*,*,#4432,.F.);
#5548=ORIENTED_EDGE('',*,*,#4433,.F.);
#5549=ORIENTED_EDGE('',*,*,#4434,.T.);
#5550=ORIENTED_EDGE('',*,*,#4435,.F.);
#5551=ORIENTED_EDGE('',*,*,#4434,.F.);
#5552=ORIENTED_EDGE('',*,*,#4433,.T.);
#5553=ORIENTED_EDGE('',*,*,#4436,.F.);
#5554=ORIENTED_EDGE('',*,*,#4437,.F.);
#5555=ORIENTED_EDGE('',*,*,#4438,.T.);
#5556=ORIENTED_EDGE('',*,*,#4439,.F.);
#5557=ORIENTED_EDGE('',*,*,#4438,.F.);
#5558=ORIENTED_EDGE('',*,*,#4437,.T.);
#5559=ORIENTED_EDGE('',*,*,#4440,.F.);
#5560=ORIENTED_EDGE('',*,*,#4441,.F.);
#5561=ORIENTED_EDGE('',*,*,#4442,.T.);
#5562=ORIENTED_EDGE('',*,*,#4428,.T.);
#5563=ORIENTED_EDGE('',*,*,#4442,.F.);
#5564=ORIENTED_EDGE('',*,*,#4443,.F.);
#5565=ORIENTED_EDGE('',*,*,#4444,.T.);
#5566=ORIENTED_EDGE('',*,*,#4432,.T.);
#5567=ORIENTED_EDGE('',*,*,#4444,.F.);
#5568=ORIENTED_EDGE('',*,*,#4445,.F.);
#5569=ORIENTED_EDGE('',*,*,#4446,.T.);
#5570=ORIENTED_EDGE('',*,*,#4436,.T.);
#5571=ORIENTED_EDGE('',*,*,#4446,.F.);
#5572=ORIENTED_EDGE('',*,*,#4447,.F.);
#5573=ORIENTED_EDGE('',*,*,#4448,.T.);
#5574=ORIENTED_EDGE('',*,*,#4440,.T.);
#5575=ORIENTED_EDGE('',*,*,#4448,.F.);
#5576=ORIENTED_EDGE('',*,*,#4449,.F.);
#5577=ORIENTED_EDGE('',*,*,#4450,.T.);
#5578=ORIENTED_EDGE('',*,*,#4451,.T.);
#5579=ORIENTED_EDGE('',*,*,#4450,.F.);
#5580=ORIENTED_EDGE('',*,*,#4451,.F.);
#5581=ORIENTED_EDGE('',*,*,#4452,.F.);
#5582=ORIENTED_EDGE('',*,*,#4453,.F.);
#5583=ORIENTED_EDGE('',*,*,#4454,.T.);
#5584=ORIENTED_EDGE('',*,*,#4452,.T.);
#5585=ORIENTED_EDGE('',*,*,#4454,.F.);
#5586=ORIENTED_EDGE('',*,*,#4455,.F.);
#5587=ORIENTED_EDGE('',*,*,#4456,.T.);
#5588=ORIENTED_EDGE('',*,*,#4457,.T.);
#5589=ORIENTED_EDGE('',*,*,#4456,.F.);
#5590=ORIENTED_EDGE('',*,*,#4455,.T.);
#5591=ORIENTED_EDGE('',*,*,#4453,.T.);
#5592=ORIENTED_EDGE('',*,*,#4439,.T.);
#5593=ORIENTED_EDGE('',*,*,#4435,.T.);
#5594=ORIENTED_EDGE('',*,*,#4431,.T.);
#5595=ORIENTED_EDGE('',*,*,#4427,.T.);
#5596=ORIENTED_EDGE('',*,*,#4457,.F.);
#5597=ORIENTED_EDGE('',*,*,#4449,.T.);
#5598=ORIENTED_EDGE('',*,*,#4447,.T.);
#5599=ORIENTED_EDGE('',*,*,#4445,.T.);
#5600=ORIENTED_EDGE('',*,*,#4443,.T.);
#5601=ORIENTED_EDGE('',*,*,#4441,.T.);
#5602=ORIENTED_EDGE('',*,*,#4458,.F.);
#5603=ORIENTED_EDGE('',*,*,#4459,.F.);
#5604=ORIENTED_EDGE('',*,*,#4460,.T.);
#5605=ORIENTED_EDGE('',*,*,#4461,.F.);
#5606=ORIENTED_EDGE('',*,*,#4462,.F.);
#5607=ORIENTED_EDGE('',*,*,#4460,.F.);
#5608=ORIENTED_EDGE('',*,*,#4463,.F.);
#5609=ORIENTED_EDGE('',*,*,#4464,.T.);
#5610=ORIENTED_EDGE('',*,*,#4465,.F.);
#5611=ORIENTED_EDGE('',*,*,#4464,.F.);
#5612=ORIENTED_EDGE('',*,*,#4463,.T.);
#5613=ORIENTED_EDGE('',*,*,#4466,.F.);
#5614=ORIENTED_EDGE('',*,*,#4467,.T.);
#5615=ORIENTED_EDGE('',*,*,#4468,.F.);
#5616=ORIENTED_EDGE('',*,*,#4467,.F.);
#5617=ORIENTED_EDGE('',*,*,#4466,.T.);
#5618=ORIENTED_EDGE('',*,*,#4469,.F.);
#5619=ORIENTED_EDGE('',*,*,#4470,.T.);
#5620=ORIENTED_EDGE('',*,*,#4471,.F.);
#5621=ORIENTED_EDGE('',*,*,#4470,.F.);
#5622=ORIENTED_EDGE('',*,*,#4469,.T.);
#5623=ORIENTED_EDGE('',*,*,#4472,.F.);
#5624=ORIENTED_EDGE('',*,*,#4473,.T.);
#5625=ORIENTED_EDGE('',*,*,#4474,.F.);
#5626=ORIENTED_EDGE('',*,*,#4473,.F.);
#5627=ORIENTED_EDGE('',*,*,#4472,.T.);
#5628=ORIENTED_EDGE('',*,*,#4475,.F.);
#5629=ORIENTED_EDGE('',*,*,#4476,.T.);
#5630=ORIENTED_EDGE('',*,*,#4477,.F.);
#5631=ORIENTED_EDGE('',*,*,#4478,.F.);
#5632=ORIENTED_EDGE('',*,*,#4479,.F.);
#5633=ORIENTED_EDGE('',*,*,#4476,.F.);
#5634=ORIENTED_EDGE('',*,*,#4480,.F.);
#5635=ORIENTED_EDGE('',*,*,#4481,.T.);
#5636=ORIENTED_EDGE('',*,*,#4482,.F.);
#5637=ORIENTED_EDGE('',*,*,#4483,.F.);
#5638=ORIENTED_EDGE('',*,*,#4484,.F.);
#5639=ORIENTED_EDGE('',*,*,#4481,.F.);
#5640=ORIENTED_EDGE('',*,*,#4485,.F.);
#5641=ORIENTED_EDGE('',*,*,#4486,.T.);
#5642=ORIENTED_EDGE('',*,*,#4487,.F.);
#5643=ORIENTED_EDGE('',*,*,#4488,.F.);
#5644=ORIENTED_EDGE('',*,*,#4489,.F.);
#5645=ORIENTED_EDGE('',*,*,#4486,.F.);
#5646=ORIENTED_EDGE('',*,*,#4490,.F.);
#5647=ORIENTED_EDGE('',*,*,#4491,.T.);
#5648=ORIENTED_EDGE('',*,*,#4492,.F.);
#5649=ORIENTED_EDGE('',*,*,#4493,.F.);
#5650=ORIENTED_EDGE('',*,*,#4494,.F.);
#5651=ORIENTED_EDGE('',*,*,#4491,.F.);
#5652=ORIENTED_EDGE('',*,*,#4495,.T.);
#5653=ORIENTED_EDGE('',*,*,#4496,.F.);
#5654=ORIENTED_EDGE('',*,*,#4483,.T.);
#5655=ORIENTED_EDGE('',*,*,#4497,.F.);
#5656=ORIENTED_EDGE('',*,*,#4488,.T.);
#5657=ORIENTED_EDGE('',*,*,#4498,.F.);
#5658=ORIENTED_EDGE('',*,*,#4493,.T.);
#5659=ORIENTED_EDGE('',*,*,#4499,.F.);
#5660=ORIENTED_EDGE('',*,*,#4478,.T.);
#5661=ORIENTED_EDGE('',*,*,#4500,.F.);
#5662=ORIENTED_EDGE('',*,*,#4501,.T.);
#5663=ORIENTED_EDGE('',*,*,#4502,.T.);
#5664=ORIENTED_EDGE('',*,*,#4503,.T.);
#5665=ORIENTED_EDGE('',*,*,#4504,.T.);
#5666=ORIENTED_EDGE('',*,*,#4505,.F.);
#5667=ORIENTED_EDGE('',*,*,#4506,.T.);
#5668=ORIENTED_EDGE('',*,*,#4501,.F.);
#5669=ORIENTED_EDGE('',*,*,#4506,.F.);
#5670=ORIENTED_EDGE('',*,*,#4507,.F.);
#5671=ORIENTED_EDGE('',*,*,#4508,.T.);
#5672=ORIENTED_EDGE('',*,*,#4502,.F.);
#5673=ORIENTED_EDGE('',*,*,#4508,.F.);
#5674=ORIENTED_EDGE('',*,*,#4509,.F.);
#5675=ORIENTED_EDGE('',*,*,#4510,.T.);
#5676=ORIENTED_EDGE('',*,*,#4503,.F.);
#5677=ORIENTED_EDGE('',*,*,#4510,.F.);
#5678=ORIENTED_EDGE('',*,*,#4511,.F.);
#5679=ORIENTED_EDGE('',*,*,#4512,.T.);
#5680=ORIENTED_EDGE('',*,*,#4504,.F.);
#5681=ORIENTED_EDGE('',*,*,#4512,.F.);
#5682=ORIENTED_EDGE('',*,*,#4513,.F.);
#5683=ORIENTED_EDGE('',*,*,#4514,.T.);
#5684=ORIENTED_EDGE('',*,*,#4500,.T.);
#5685=ORIENTED_EDGE('',*,*,#4477,.T.);
#5686=ORIENTED_EDGE('',*,*,#4479,.T.);
#5687=ORIENTED_EDGE('',*,*,#4475,.T.);
#5688=ORIENTED_EDGE('',*,*,#4499,.T.);
#5689=ORIENTED_EDGE('',*,*,#4492,.T.);
#5690=ORIENTED_EDGE('',*,*,#4494,.T.);
#5691=ORIENTED_EDGE('',*,*,#4490,.T.);
#5692=ORIENTED_EDGE('',*,*,#4498,.T.);
#5693=ORIENTED_EDGE('',*,*,#4487,.T.);
#5694=ORIENTED_EDGE('',*,*,#4489,.T.);
#5695=ORIENTED_EDGE('',*,*,#4485,.T.);
#5696=ORIENTED_EDGE('',*,*,#4497,.T.);
#5697=ORIENTED_EDGE('',*,*,#4482,.T.);
#5698=ORIENTED_EDGE('',*,*,#4484,.T.);
#5699=ORIENTED_EDGE('',*,*,#4480,.T.);
#5700=ORIENTED_EDGE('',*,*,#4496,.T.);
#5701=ORIENTED_EDGE('',*,*,#4514,.F.);
#5702=ORIENTED_EDGE('',*,*,#4515,.F.);
#5703=ORIENTED_EDGE('',*,*,#4516,.T.);
#5704=ORIENTED_EDGE('',*,*,#4517,.F.);
#5705=ORIENTED_EDGE('',*,*,#4516,.F.);
#5706=ORIENTED_EDGE('',*,*,#4515,.T.);
#5707=ORIENTED_EDGE('',*,*,#4518,.F.);
#5708=ORIENTED_EDGE('',*,*,#4495,.F.);
#5709=ORIENTED_EDGE('',*,*,#4519,.T.);
#5710=ORIENTED_EDGE('',*,*,#4520,.T.);
#5711=ORIENTED_EDGE('',*,*,#4519,.F.);
#5712=ORIENTED_EDGE('',*,*,#4461,.T.);
#5713=ORIENTED_EDGE('',*,*,#4462,.T.);
#5714=ORIENTED_EDGE('',*,*,#4518,.T.);
#5715=ORIENTED_EDGE('',*,*,#4521,.T.);
#5716=ORIENTED_EDGE('',*,*,#4522,.T.);
#5717=ORIENTED_EDGE('',*,*,#4521,.F.);
#5718=ORIENTED_EDGE('',*,*,#4458,.T.);
#5719=ORIENTED_EDGE('',*,*,#4459,.T.);
#5720=ORIENTED_EDGE('',*,*,#4513,.T.);
#5721=ORIENTED_EDGE('',*,*,#4517,.T.);
#5722=ORIENTED_EDGE('',*,*,#4474,.T.);
#5723=ORIENTED_EDGE('',*,*,#4471,.T.);
#5724=ORIENTED_EDGE('',*,*,#4468,.T.);
#5725=ORIENTED_EDGE('',*,*,#4465,.T.);
#5726=ORIENTED_EDGE('',*,*,#4520,.F.);
#5727=ORIENTED_EDGE('',*,*,#4522,.F.);
#5728=ORIENTED_EDGE('',*,*,#4511,.T.);
#5729=ORIENTED_EDGE('',*,*,#4509,.T.);
#5730=ORIENTED_EDGE('',*,*,#4507,.T.);
#5731=ORIENTED_EDGE('',*,*,#4505,.T.);
#5732=ORIENTED_EDGE('',*,*,#4523,.F.);
#5733=ORIENTED_EDGE('',*,*,#4524,.T.);
#5734=ORIENTED_EDGE('',*,*,#4525,.F.);
#5735=ORIENTED_EDGE('',*,*,#4524,.F.);
#5736=ORIENTED_EDGE('',*,*,#4523,.T.);
#5737=ORIENTED_EDGE('',*,*,#4526,.F.);
#5738=ORIENTED_EDGE('',*,*,#4527,.F.);
#5739=ORIENTED_EDGE('',*,*,#4528,.T.);
#5740=ORIENTED_EDGE('',*,*,#4529,.F.);
#5741=ORIENTED_EDGE('',*,*,#4528,.F.);
#5742=ORIENTED_EDGE('',*,*,#4527,.T.);
#5743=ORIENTED_EDGE('',*,*,#4530,.F.);
#5744=ORIENTED_EDGE('',*,*,#4531,.F.);
#5745=ORIENTED_EDGE('',*,*,#4532,.T.);
#5746=ORIENTED_EDGE('',*,*,#4533,.F.);
#5747=ORIENTED_EDGE('',*,*,#4532,.F.);
#5748=ORIENTED_EDGE('',*,*,#4531,.T.);
#5749=ORIENTED_EDGE('',*,*,#4534,.F.);
#5750=ORIENTED_EDGE('',*,*,#4535,.F.);
#5751=ORIENTED_EDGE('',*,*,#4536,.T.);
#5752=ORIENTED_EDGE('',*,*,#4537,.F.);
#5753=ORIENTED_EDGE('',*,*,#4536,.F.);
#5754=ORIENTED_EDGE('',*,*,#4535,.T.);
#5755=ORIENTED_EDGE('',*,*,#4538,.F.);
#5756=ORIENTED_EDGE('',*,*,#4539,.F.);
#5757=ORIENTED_EDGE('',*,*,#4540,.T.);
#5758=ORIENTED_EDGE('',*,*,#4526,.T.);
#5759=ORIENTED_EDGE('',*,*,#4540,.F.);
#5760=ORIENTED_EDGE('',*,*,#4541,.F.);
#5761=ORIENTED_EDGE('',*,*,#4542,.T.);
#5762=ORIENTED_EDGE('',*,*,#4530,.T.);
#5763=ORIENTED_EDGE('',*,*,#4542,.F.);
#5764=ORIENTED_EDGE('',*,*,#4543,.F.);
#5765=ORIENTED_EDGE('',*,*,#4544,.T.);
#5766=ORIENTED_EDGE('',*,*,#4534,.T.);
#5767=ORIENTED_EDGE('',*,*,#4544,.F.);
#5768=ORIENTED_EDGE('',*,*,#4545,.F.);
#5769=ORIENTED_EDGE('',*,*,#4546,.T.);
#5770=ORIENTED_EDGE('',*,*,#4538,.T.);
#5771=ORIENTED_EDGE('',*,*,#4546,.F.);
#5772=ORIENTED_EDGE('',*,*,#4547,.F.);
#5773=ORIENTED_EDGE('',*,*,#4548,.T.);
#5774=ORIENTED_EDGE('',*,*,#4549,.T.);
#5775=ORIENTED_EDGE('',*,*,#4548,.F.);
#5776=ORIENTED_EDGE('',*,*,#4549,.F.);
#5777=ORIENTED_EDGE('',*,*,#4550,.F.);
#5778=ORIENTED_EDGE('',*,*,#4551,.F.);
#5779=ORIENTED_EDGE('',*,*,#4552,.T.);
#5780=ORIENTED_EDGE('',*,*,#4550,.T.);
#5781=ORIENTED_EDGE('',*,*,#4552,.F.);
#5782=ORIENTED_EDGE('',*,*,#4553,.F.);
#5783=ORIENTED_EDGE('',*,*,#4554,.T.);
#5784=ORIENTED_EDGE('',*,*,#4555,.T.);
#5785=ORIENTED_EDGE('',*,*,#4554,.F.);
#5786=ORIENTED_EDGE('',*,*,#4553,.T.);
#5787=ORIENTED_EDGE('',*,*,#4551,.T.);
#5788=ORIENTED_EDGE('',*,*,#4537,.T.);
#5789=ORIENTED_EDGE('',*,*,#4533,.T.);
#5790=ORIENTED_EDGE('',*,*,#4529,.T.);
#5791=ORIENTED_EDGE('',*,*,#4525,.T.);
#5792=ORIENTED_EDGE('',*,*,#4555,.F.);
#5793=ORIENTED_EDGE('',*,*,#4547,.T.);
#5794=ORIENTED_EDGE('',*,*,#4545,.T.);
#5795=ORIENTED_EDGE('',*,*,#4543,.T.);
#5796=ORIENTED_EDGE('',*,*,#4541,.T.);
#5797=ORIENTED_EDGE('',*,*,#4539,.T.);
#5798=ORIENTED_EDGE('',*,*,#4556,.F.);
#5799=ORIENTED_EDGE('',*,*,#4557,.T.);
#5800=ORIENTED_EDGE('',*,*,#4558,.F.);
#5801=ORIENTED_EDGE('',*,*,#4557,.F.);
#5802=ORIENTED_EDGE('',*,*,#4556,.T.);
#5803=ORIENTED_EDGE('',*,*,#4559,.F.);
#5804=ORIENTED_EDGE('',*,*,#4560,.F.);
#5805=ORIENTED_EDGE('',*,*,#4561,.T.);
#5806=ORIENTED_EDGE('',*,*,#4562,.F.);
#5807=ORIENTED_EDGE('',*,*,#4561,.F.);
#5808=ORIENTED_EDGE('',*,*,#4560,.T.);
#5809=ORIENTED_EDGE('',*,*,#4563,.F.);
#5810=ORIENTED_EDGE('',*,*,#4564,.F.);
#5811=ORIENTED_EDGE('',*,*,#4565,.T.);
#5812=ORIENTED_EDGE('',*,*,#4566,.F.);
#5813=ORIENTED_EDGE('',*,*,#4565,.F.);
#5814=ORIENTED_EDGE('',*,*,#4564,.T.);
#5815=ORIENTED_EDGE('',*,*,#4567,.F.);
#5816=ORIENTED_EDGE('',*,*,#4568,.F.);
#5817=ORIENTED_EDGE('',*,*,#4569,.T.);
#5818=ORIENTED_EDGE('',*,*,#4570,.F.);
#5819=ORIENTED_EDGE('',*,*,#4569,.F.);
#5820=ORIENTED_EDGE('',*,*,#4568,.T.);
#5821=ORIENTED_EDGE('',*,*,#4571,.F.);
#5822=ORIENTED_EDGE('',*,*,#4572,.F.);
#5823=ORIENTED_EDGE('',*,*,#4573,.T.);
#5824=ORIENTED_EDGE('',*,*,#4559,.T.);
#5825=ORIENTED_EDGE('',*,*,#4573,.F.);
#5826=ORIENTED_EDGE('',*,*,#4574,.F.);
#5827=ORIENTED_EDGE('',*,*,#4575,.T.);
#5828=ORIENTED_EDGE('',*,*,#4563,.T.);
#5829=ORIENTED_EDGE('',*,*,#4575,.F.);
#5830=ORIENTED_EDGE('',*,*,#4576,.F.);
#5831=ORIENTED_EDGE('',*,*,#4577,.T.);
#5832=ORIENTED_EDGE('',*,*,#4567,.T.);
#5833=ORIENTED_EDGE('',*,*,#4577,.F.);
#5834=ORIENTED_EDGE('',*,*,#4578,.F.);
#5835=ORIENTED_EDGE('',*,*,#4579,.T.);
#5836=ORIENTED_EDGE('',*,*,#4571,.T.);
#5837=ORIENTED_EDGE('',*,*,#4579,.F.);
#5838=ORIENTED_EDGE('',*,*,#4580,.T.);
#5839=ORIENTED_EDGE('',*,*,#4581,.T.);
#5840=ORIENTED_EDGE('',*,*,#4582,.F.);
#5841=ORIENTED_EDGE('',*,*,#4583,.F.);
#5842=ORIENTED_EDGE('',*,*,#4584,.T.);
#5843=ORIENTED_EDGE('',*,*,#4583,.T.);
#5844=ORIENTED_EDGE('',*,*,#4585,.F.);
#5845=ORIENTED_EDGE('',*,*,#4586,.F.);
#5846=ORIENTED_EDGE('',*,*,#4587,.T.);
#5847=ORIENTED_EDGE('',*,*,#4586,.T.);
#5848=ORIENTED_EDGE('',*,*,#4588,.F.);
#5849=ORIENTED_EDGE('',*,*,#4589,.F.);
#5850=ORIENTED_EDGE('',*,*,#4590,.T.);
#5851=ORIENTED_EDGE('',*,*,#4589,.T.);
#5852=ORIENTED_EDGE('',*,*,#4591,.F.);
#5853=ORIENTED_EDGE('',*,*,#4592,.F.);
#5854=ORIENTED_EDGE('',*,*,#4593,.T.);
#5855=ORIENTED_EDGE('',*,*,#4592,.T.);
#5856=ORIENTED_EDGE('',*,*,#4594,.F.);
#5857=ORIENTED_EDGE('',*,*,#4595,.F.);
#5858=ORIENTED_EDGE('',*,*,#4570,.T.);
#5859=ORIENTED_EDGE('',*,*,#4566,.T.);
#5860=ORIENTED_EDGE('',*,*,#4562,.T.);
#5861=ORIENTED_EDGE('',*,*,#4558,.T.);
#5862=ORIENTED_EDGE('',*,*,#4596,.T.);
#5863=ORIENTED_EDGE('',*,*,#4595,.T.);
#5864=ORIENTED_EDGE('',*,*,#4597,.F.);
#5865=ORIENTED_EDGE('',*,*,#4598,.F.);
#5866=ORIENTED_EDGE('',*,*,#4599,.T.);
#5867=ORIENTED_EDGE('',*,*,#4598,.T.);
#5868=ORIENTED_EDGE('',*,*,#4600,.F.);
#5869=ORIENTED_EDGE('',*,*,#4601,.F.);
#5870=ORIENTED_EDGE('',*,*,#4602,.T.);
#5871=ORIENTED_EDGE('',*,*,#4601,.T.);
#5872=ORIENTED_EDGE('',*,*,#4603,.F.);
#5873=ORIENTED_EDGE('',*,*,#4604,.F.);
#5874=ORIENTED_EDGE('',*,*,#4605,.T.);
#5875=ORIENTED_EDGE('',*,*,#4604,.T.);
#5876=ORIENTED_EDGE('',*,*,#4606,.F.);
#5877=ORIENTED_EDGE('',*,*,#4607,.F.);
#5878=ORIENTED_EDGE('',*,*,#4608,.T.);
#5879=ORIENTED_EDGE('',*,*,#4607,.T.);
#5880=ORIENTED_EDGE('',*,*,#4609,.F.);
#5881=ORIENTED_EDGE('',*,*,#4610,.F.);
#5882=ORIENTED_EDGE('',*,*,#4611,.T.);
#5883=ORIENTED_EDGE('',*,*,#4610,.T.);
#5884=ORIENTED_EDGE('',*,*,#4612,.F.);
#5885=ORIENTED_EDGE('',*,*,#4613,.F.);
#5886=ORIENTED_EDGE('',*,*,#4572,.T.);
#5887=ORIENTED_EDGE('',*,*,#4574,.T.);
#5888=ORIENTED_EDGE('',*,*,#4576,.T.);
#5889=ORIENTED_EDGE('',*,*,#4578,.T.);
#5890=ORIENTED_EDGE('',*,*,#4614,.T.);
#5891=ORIENTED_EDGE('',*,*,#4613,.T.);
#5892=ORIENTED_EDGE('',*,*,#4615,.F.);
#5893=ORIENTED_EDGE('',*,*,#4581,.F.);
#5894=ORIENTED_EDGE('',*,*,#4615,.T.);
#5895=ORIENTED_EDGE('',*,*,#4612,.T.);
#5896=ORIENTED_EDGE('',*,*,#4609,.T.);
#5897=ORIENTED_EDGE('',*,*,#4606,.T.);
#5898=ORIENTED_EDGE('',*,*,#4603,.T.);
#5899=ORIENTED_EDGE('',*,*,#4600,.T.);
#5900=ORIENTED_EDGE('',*,*,#4597,.T.);
#5901=ORIENTED_EDGE('',*,*,#4594,.T.);
#5902=ORIENTED_EDGE('',*,*,#4591,.T.);
#5903=ORIENTED_EDGE('',*,*,#4588,.T.);
#5904=ORIENTED_EDGE('',*,*,#4585,.T.);
#5905=ORIENTED_EDGE('',*,*,#4582,.T.);
#5906=ORIENTED_EDGE('',*,*,#4614,.F.);
#5907=ORIENTED_EDGE('',*,*,#4580,.F.);
#5908=ORIENTED_EDGE('',*,*,#4584,.F.);
#5909=ORIENTED_EDGE('',*,*,#4587,.F.);
#5910=ORIENTED_EDGE('',*,*,#4590,.F.);
#5911=ORIENTED_EDGE('',*,*,#4593,.F.);
#5912=ORIENTED_EDGE('',*,*,#4596,.F.);
#5913=ORIENTED_EDGE('',*,*,#4599,.F.);
#5914=ORIENTED_EDGE('',*,*,#4602,.F.);
#5915=ORIENTED_EDGE('',*,*,#4605,.F.);
#5916=ORIENTED_EDGE('',*,*,#4608,.F.);
#5917=ORIENTED_EDGE('',*,*,#4611,.F.);
#5918=ORIENTED_EDGE('',*,*,#4616,.F.);
#5919=ORIENTED_EDGE('',*,*,#4617,.F.);
#5920=ORIENTED_EDGE('',*,*,#4618,.T.);
#5921=ORIENTED_EDGE('',*,*,#4619,.F.);
#5922=ORIENTED_EDGE('',*,*,#4620,.F.);
#5923=ORIENTED_EDGE('',*,*,#4618,.F.);
#5924=ORIENTED_EDGE('',*,*,#4619,.T.);
#5925=ORIENTED_EDGE('',*,*,#4620,.T.);
#5926=ORIENTED_EDGE('',*,*,#4621,.T.);
#5927=ORIENTED_EDGE('',*,*,#4622,.T.);
#5928=ORIENTED_EDGE('',*,*,#4621,.F.);
#5929=ORIENTED_EDGE('',*,*,#4623,.T.);
#5930=ORIENTED_EDGE('',*,*,#4624,.T.);
#5931=ORIENTED_EDGE('',*,*,#4625,.F.);
#5932=ORIENTED_EDGE('',*,*,#4624,.F.);
#5933=ORIENTED_EDGE('',*,*,#4625,.T.);
#5934=ORIENTED_EDGE('',*,*,#4626,.T.);
#5935=ORIENTED_EDGE('',*,*,#4627,.F.);
#5936=ORIENTED_EDGE('',*,*,#4626,.F.);
#5937=ORIENTED_EDGE('',*,*,#4622,.F.);
#5938=ORIENTED_EDGE('',*,*,#4627,.T.);
#5939=ORIENTED_EDGE('',*,*,#4628,.F.);
#5940=ORIENTED_EDGE('',*,*,#4629,.T.);
#5941=ORIENTED_EDGE('',*,*,#4616,.T.);
#5942=ORIENTED_EDGE('',*,*,#4617,.T.);
#5943=ORIENTED_EDGE('',*,*,#4629,.F.);
#5944=ORIENTED_EDGE('',*,*,#4628,.T.);
#5945=ORIENTED_EDGE('',*,*,#4630,.F.);
#5946=ORIENTED_EDGE('',*,*,#4630,.T.);
#5947=ORIENTED_EDGE('',*,*,#4631,.T.);
#5948=ORIENTED_EDGE('',*,*,#4623,.F.);
#5949=ORIENTED_EDGE('',*,*,#4631,.F.);
#5950=ORIENTED_EDGE('',*,*,#4632,.F.);
#5951=ORIENTED_EDGE('',*,*,#4633,.F.);
#5952=ORIENTED_EDGE('',*,*,#4634,.T.);
#5953=ORIENTED_EDGE('',*,*,#4635,.F.);
#5954=ORIENTED_EDGE('',*,*,#4636,.F.);
#5955=ORIENTED_EDGE('',*,*,#4634,.F.);
#5956=ORIENTED_EDGE('',*,*,#4637,.T.);
#5957=ORIENTED_EDGE('',*,*,#4638,.T.);
#5958=ORIENTED_EDGE('',*,*,#4635,.T.);
#5959=ORIENTED_EDGE('',*,*,#4636,.T.);
#5960=ORIENTED_EDGE('',*,*,#4638,.F.);
#5961=ORIENTED_EDGE('',*,*,#4639,.F.);
#5962=ORIENTED_EDGE('',*,*,#4640,.T.);
#5963=ORIENTED_EDGE('',*,*,#4641,.F.);
#5964=ORIENTED_EDGE('',*,*,#4642,.T.);
#5965=ORIENTED_EDGE('',*,*,#4639,.T.);
#5966=ORIENTED_EDGE('',*,*,#4642,.F.);
#5967=ORIENTED_EDGE('',*,*,#4643,.F.);
#5968=ORIENTED_EDGE('',*,*,#4644,.T.);
#5969=ORIENTED_EDGE('',*,*,#4641,.T.);
#5970=ORIENTED_EDGE('',*,*,#4644,.F.);
#5971=ORIENTED_EDGE('',*,*,#4645,.F.);
#5972=ORIENTED_EDGE('',*,*,#4646,.T.);
#5973=ORIENTED_EDGE('',*,*,#4643,.T.);
#5974=ORIENTED_EDGE('',*,*,#4646,.F.);
#5975=ORIENTED_EDGE('',*,*,#4645,.T.);
#5976=ORIENTED_EDGE('',*,*,#4637,.F.);
#5977=ORIENTED_EDGE('',*,*,#4632,.T.);
#5978=ORIENTED_EDGE('',*,*,#4633,.T.);
#5979=ORIENTED_EDGE('',*,*,#4647,.T.);
#5980=ORIENTED_EDGE('',*,*,#4640,.F.);
#5981=ORIENTED_EDGE('',*,*,#4647,.F.);
#5982=ORIENTED_EDGE('',*,*,#4648,.T.);
#5983=ORIENTED_EDGE('',*,*,#4648,.F.);
#5984=ORIENTED_EDGE('',*,*,#4649,.T.);
#5985=ORIENTED_EDGE('',*,*,#4649,.F.);
#5986=ORIENTED_EDGE('',*,*,#4650,.T.);
#5987=ORIENTED_EDGE('',*,*,#4650,.F.);
#5988=ORIENTED_EDGE('',*,*,#4651,.T.);
#5989=ORIENTED_EDGE('',*,*,#4651,.F.);
#5990=ORIENTED_EDGE('',*,*,#4652,.T.);
#5991=ORIENTED_EDGE('',*,*,#4652,.F.);
#5992=ORIENTED_EDGE('',*,*,#4653,.T.);
#5993=ORIENTED_EDGE('',*,*,#4653,.F.);
#5994=ORIENTED_EDGE('',*,*,#4654,.T.);
#5995=ORIENTED_EDGE('',*,*,#4654,.F.);
#5996=ORIENTED_EDGE('',*,*,#4655,.T.);
#5997=ORIENTED_EDGE('',*,*,#4655,.F.);
#5998=ORIENTED_EDGE('',*,*,#4656,.F.);
#5999=ORIENTED_EDGE('',*,*,#4657,.F.);
#6000=ORIENTED_EDGE('',*,*,#4658,.F.);
#6001=ORIENTED_EDGE('',*,*,#4659,.F.);
#6002=ORIENTED_EDGE('',*,*,#4658,.T.);
#6003=ORIENTED_EDGE('',*,*,#4660,.F.);
#6004=ORIENTED_EDGE('',*,*,#4661,.T.);
#6005=ORIENTED_EDGE('',*,*,#4662,.F.);
#6006=ORIENTED_EDGE('',*,*,#4663,.T.);
#6007=ORIENTED_EDGE('',*,*,#4664,.F.);
#6008=ORIENTED_EDGE('',*,*,#4665,.T.);
#6009=ORIENTED_EDGE('',*,*,#4666,.T.);
#6010=ORIENTED_EDGE('',*,*,#4667,.F.);
#6011=ORIENTED_EDGE('',*,*,#4666,.F.);
#6012=ORIENTED_EDGE('',*,*,#4668,.T.);
#6013=ORIENTED_EDGE('',*,*,#4669,.F.);
#6014=ORIENTED_EDGE('',*,*,#4670,.T.);
#6015=ORIENTED_EDGE('',*,*,#4671,.F.);
#6016=ORIENTED_EDGE('',*,*,#4672,.T.);
#6017=ORIENTED_EDGE('',*,*,#4673,.F.);
#6018=ORIENTED_EDGE('',*,*,#4674,.T.);
#6019=ORIENTED_EDGE('',*,*,#4675,.F.);
#6020=ORIENTED_EDGE('',*,*,#4676,.T.);
#6021=ORIENTED_EDGE('',*,*,#4677,.F.);
#6022=ORIENTED_EDGE('',*,*,#4657,.T.);
#6023=ORIENTED_EDGE('',*,*,#4678,.T.);
#6024=ORIENTED_EDGE('',*,*,#4679,.T.);
#6025=ORIENTED_EDGE('',*,*,#4660,.T.);
#6026=ORIENTED_EDGE('',*,*,#4680,.F.);
#6027=ORIENTED_EDGE('',*,*,#4681,.F.);
#6028=ORIENTED_EDGE('',*,*,#4661,.F.);
#6029=ORIENTED_EDGE('',*,*,#4679,.F.);
#6030=ORIENTED_EDGE('',*,*,#4681,.T.);
#6031=ORIENTED_EDGE('',*,*,#4682,.T.);
#6032=ORIENTED_EDGE('',*,*,#4683,.T.);
#6033=ORIENTED_EDGE('',*,*,#4662,.T.);
#6034=ORIENTED_EDGE('',*,*,#4684,.F.);
#6035=ORIENTED_EDGE('',*,*,#4685,.F.);
#6036=ORIENTED_EDGE('',*,*,#4663,.F.);
#6037=ORIENTED_EDGE('',*,*,#4683,.F.);
#6038=ORIENTED_EDGE('',*,*,#4685,.T.);
#6039=ORIENTED_EDGE('',*,*,#4686,.T.);
#6040=ORIENTED_EDGE('',*,*,#4687,.T.);
#6041=ORIENTED_EDGE('',*,*,#4664,.T.);
#6042=ORIENTED_EDGE('',*,*,#4688,.F.);
#6043=ORIENTED_EDGE('',*,*,#4689,.F.);
#6044=ORIENTED_EDGE('',*,*,#4668,.F.);
#6045=ORIENTED_EDGE('',*,*,#4665,.F.);
#6046=ORIENTED_EDGE('',*,*,#4687,.F.);
#6047=ORIENTED_EDGE('',*,*,#4690,.F.);
#6048=ORIENTED_EDGE('',*,*,#4689,.T.);
#6049=ORIENTED_EDGE('',*,*,#4691,.T.);
#6050=ORIENTED_EDGE('',*,*,#4692,.T.);
#6051=ORIENTED_EDGE('',*,*,#4669,.T.);
#6052=ORIENTED_EDGE('',*,*,#4693,.F.);
#6053=ORIENTED_EDGE('',*,*,#4694,.F.);
#6054=ORIENTED_EDGE('',*,*,#4670,.F.);
#6055=ORIENTED_EDGE('',*,*,#4692,.F.);
#6056=ORIENTED_EDGE('',*,*,#4694,.T.);
#6057=ORIENTED_EDGE('',*,*,#4695,.T.);
#6058=ORIENTED_EDGE('',*,*,#4696,.T.);
#6059=ORIENTED_EDGE('',*,*,#4671,.T.);
#6060=ORIENTED_EDGE('',*,*,#4697,.F.);
#6061=ORIENTED_EDGE('',*,*,#4698,.F.);
#6062=ORIENTED_EDGE('',*,*,#4672,.F.);
#6063=ORIENTED_EDGE('',*,*,#4696,.F.);
#6064=ORIENTED_EDGE('',*,*,#4698,.T.);
#6065=ORIENTED_EDGE('',*,*,#4699,.T.);
#6066=ORIENTED_EDGE('',*,*,#4700,.T.);
#6067=ORIENTED_EDGE('',*,*,#4673,.T.);
#6068=ORIENTED_EDGE('',*,*,#4674,.F.);
#6069=ORIENTED_EDGE('',*,*,#4700,.F.);
#6070=ORIENTED_EDGE('',*,*,#4701,.F.);
#6071=ORIENTED_EDGE('',*,*,#4702,.F.);
#6072=ORIENTED_EDGE('',*,*,#4703,.F.);
#6073=ORIENTED_EDGE('',*,*,#4704,.T.);
#6074=ORIENTED_EDGE('',*,*,#4690,.T.);
#6075=ORIENTED_EDGE('',*,*,#4686,.F.);
#6076=ORIENTED_EDGE('',*,*,#4684,.T.);
#6077=ORIENTED_EDGE('',*,*,#4682,.F.);
#6078=ORIENTED_EDGE('',*,*,#4680,.T.);
#6079=ORIENTED_EDGE('',*,*,#4678,.F.);
#6080=ORIENTED_EDGE('',*,*,#4656,.T.);
#6081=ORIENTED_EDGE('',*,*,#4705,.F.);
#6082=ORIENTED_EDGE('',*,*,#4706,.T.);
#6083=ORIENTED_EDGE('',*,*,#4707,.F.);
#6084=ORIENTED_EDGE('',*,*,#4701,.T.);
#6085=ORIENTED_EDGE('',*,*,#4699,.F.);
#6086=ORIENTED_EDGE('',*,*,#4697,.T.);
#6087=ORIENTED_EDGE('',*,*,#4695,.F.);
#6088=ORIENTED_EDGE('',*,*,#4693,.T.);
#6089=ORIENTED_EDGE('',*,*,#4691,.F.);
#6090=ORIENTED_EDGE('',*,*,#4688,.T.);
#6091=ORIENTED_EDGE('',*,*,#4704,.F.);
#6092=ORIENTED_EDGE('',*,*,#4659,.T.);
#6093=ORIENTED_EDGE('',*,*,#4677,.T.);
#6094=ORIENTED_EDGE('',*,*,#4708,.T.);
#6095=ORIENTED_EDGE('',*,*,#4705,.T.);
#6096=ORIENTED_EDGE('',*,*,#4676,.F.);
#6097=ORIENTED_EDGE('',*,*,#4709,.F.);
#6098=ORIENTED_EDGE('',*,*,#4706,.F.);
#6099=ORIENTED_EDGE('',*,*,#4708,.F.);
#6100=ORIENTED_EDGE('',*,*,#4667,.T.);
#6101=ORIENTED_EDGE('',*,*,#4703,.T.);
#6102=ORIENTED_EDGE('',*,*,#4702,.T.);
#6103=ORIENTED_EDGE('',*,*,#4707,.T.);
#6104=ORIENTED_EDGE('',*,*,#4709,.T.);
#6105=ORIENTED_EDGE('',*,*,#4675,.T.);
#6106=ORIENTED_EDGE('',*,*,#4710,.F.);
#6107=ORIENTED_EDGE('',*,*,#4711,.T.);
#6108=ORIENTED_EDGE('',*,*,#4712,.F.);
#6109=ORIENTED_EDGE('',*,*,#4713,.T.);
#6110=ORIENTED_EDGE('',*,*,#4710,.T.);
#6111=ORIENTED_EDGE('',*,*,#4713,.F.);
#6112=ORIENTED_EDGE('',*,*,#4712,.T.);
#6113=ORIENTED_EDGE('',*,*,#4714,.F.);
#6114=ORIENTED_EDGE('',*,*,#4714,.T.);
#6115=ORIENTED_EDGE('',*,*,#4715,.T.);
#6116=ORIENTED_EDGE('',*,*,#4711,.F.);
#6117=ORIENTED_EDGE('',*,*,#4715,.F.);
#6118=ORIENTED_EDGE('',*,*,#4716,.F.);
#6119=ORIENTED_EDGE('',*,*,#4717,.T.);
#6120=ORIENTED_EDGE('',*,*,#4718,.F.);
#6121=ORIENTED_EDGE('',*,*,#4719,.T.);
#6122=ORIENTED_EDGE('',*,*,#4716,.T.);
#6123=ORIENTED_EDGE('',*,*,#4719,.F.);
#6124=ORIENTED_EDGE('',*,*,#4718,.T.);
#6125=ORIENTED_EDGE('',*,*,#4720,.F.);
#6126=ORIENTED_EDGE('',*,*,#4720,.T.);
#6127=ORIENTED_EDGE('',*,*,#4721,.T.);
#6128=ORIENTED_EDGE('',*,*,#4717,.F.);
#6129=ORIENTED_EDGE('',*,*,#4721,.F.);
#6130=ORIENTED_EDGE('',*,*,#4722,.F.);
#6131=ORIENTED_EDGE('',*,*,#4723,.T.);
#6132=ORIENTED_EDGE('',*,*,#4724,.F.);
#6133=ORIENTED_EDGE('',*,*,#4723,.F.);
#6134=ORIENTED_EDGE('',*,*,#4725,.F.);
#6135=ORIENTED_EDGE('',*,*,#4726,.F.);
#6136=ORIENTED_EDGE('',*,*,#4727,.F.);
#6137=ORIENTED_EDGE('',*,*,#4728,.T.);
#6138=ORIENTED_EDGE('',*,*,#4725,.T.);
#6139=ORIENTED_EDGE('',*,*,#4729,.F.);
#6140=ORIENTED_EDGE('',*,*,#4730,.F.);
#6141=ORIENTED_EDGE('',*,*,#4731,.F.);
#6142=ORIENTED_EDGE('',*,*,#4728,.F.);
#6143=ORIENTED_EDGE('',*,*,#4732,.T.);
#6144=ORIENTED_EDGE('',*,*,#4733,.F.);
#6145=ORIENTED_EDGE('',*,*,#4734,.T.);
#6146=ORIENTED_EDGE('',*,*,#4735,.F.);
#6147=ORIENTED_EDGE('',*,*,#4736,.T.);
#6148=ORIENTED_EDGE('',*,*,#4737,.F.);
#6149=ORIENTED_EDGE('',*,*,#4729,.T.);
#6150=ORIENTED_EDGE('',*,*,#4722,.T.);
#6151=ORIENTED_EDGE('',*,*,#4738,.T.);
#6152=ORIENTED_EDGE('',*,*,#4739,.T.);
#6153=ORIENTED_EDGE('',*,*,#4727,.T.);
#6154=ORIENTED_EDGE('',*,*,#4740,.F.);
#6155=ORIENTED_EDGE('',*,*,#4741,.F.);
#6156=ORIENTED_EDGE('',*,*,#4732,.F.);
#6157=ORIENTED_EDGE('',*,*,#4741,.T.);
#6158=ORIENTED_EDGE('',*,*,#4742,.F.);
#6159=ORIENTED_EDGE('',*,*,#4743,.T.);
#6160=ORIENTED_EDGE('',*,*,#4733,.T.);
#6161=ORIENTED_EDGE('',*,*,#4738,.F.);
#6162=ORIENTED_EDGE('',*,*,#4744,.T.);
#6163=ORIENTED_EDGE('',*,*,#4745,.F.);
#6164=ORIENTED_EDGE('',*,*,#4744,.F.);
#6165=ORIENTED_EDGE('',*,*,#4746,.F.);
#6166=ORIENTED_EDGE('',*,*,#4735,.T.);
#6167=ORIENTED_EDGE('',*,*,#4747,.F.);
#6168=ORIENTED_EDGE('',*,*,#4748,.F.);
#6169=ORIENTED_EDGE('',*,*,#4746,.T.);
#6170=ORIENTED_EDGE('',*,*,#4749,.F.);
#6171=ORIENTED_EDGE('',*,*,#4750,.F.);
#6172=ORIENTED_EDGE('',*,*,#4736,.F.);
#6173=ORIENTED_EDGE('',*,*,#4731,.T.);
#6174=ORIENTED_EDGE('',*,*,#4751,.T.);
#6175=ORIENTED_EDGE('',*,*,#4749,.T.);
#6176=ORIENTED_EDGE('',*,*,#4748,.T.);
#6177=ORIENTED_EDGE('',*,*,#4752,.T.);
#6178=ORIENTED_EDGE('',*,*,#4742,.T.);
#6179=ORIENTED_EDGE('',*,*,#4740,.T.);
#6180=ORIENTED_EDGE('',*,*,#4726,.T.);
#6181=ORIENTED_EDGE('',*,*,#4724,.T.);
#6182=ORIENTED_EDGE('',*,*,#4745,.T.);
#6183=ORIENTED_EDGE('',*,*,#4747,.T.);
#6184=ORIENTED_EDGE('',*,*,#4734,.F.);
#6185=ORIENTED_EDGE('',*,*,#4743,.F.);
#6186=ORIENTED_EDGE('',*,*,#4752,.F.);
#6187=ORIENTED_EDGE('',*,*,#4730,.T.);
#6188=ORIENTED_EDGE('',*,*,#4737,.T.);
#6189=ORIENTED_EDGE('',*,*,#4750,.T.);
#6190=ORIENTED_EDGE('',*,*,#4751,.F.);
#6191=ORIENTED_EDGE('',*,*,#4753,.F.);
#6192=ORIENTED_EDGE('',*,*,#4754,.F.);
#6193=ORIENTED_EDGE('',*,*,#4739,.F.);
#6194=ORIENTED_EDGE('',*,*,#4755,.T.);
#6195=ORIENTED_EDGE('',*,*,#4753,.T.);
#6196=ORIENTED_EDGE('',*,*,#4755,.F.);
#6197=ORIENTED_EDGE('',*,*,#4754,.T.);
#6198=ORIENTED_EDGE('',*,*,#4756,.T.);
#6199=ORIENTED_EDGE('',*,*,#4757,.T.);
#6200=ORIENTED_EDGE('',*,*,#4756,.F.);
#6201=ORIENTED_EDGE('',*,*,#4757,.F.);
#6202=ORIENTED_EDGE('',*,*,#4758,.F.);
#6203=ORIENTED_EDGE('',*,*,#4759,.T.);
#6204=ORIENTED_EDGE('',*,*,#4760,.F.);
#6205=ORIENTED_EDGE('',*,*,#4759,.F.);
#6206=ORIENTED_EDGE('',*,*,#4758,.T.);
#6207=ORIENTED_EDGE('',*,*,#4761,.F.);
#6208=ORIENTED_EDGE('',*,*,#4762,.T.);
#6209=ORIENTED_EDGE('',*,*,#4763,.T.);
#6210=ORIENTED_EDGE('',*,*,#4762,.F.);
#6211=ORIENTED_EDGE('',*,*,#4761,.T.);
#6212=ORIENTED_EDGE('',*,*,#4760,.T.);
#6213=ORIENTED_EDGE('',*,*,#4763,.F.);
#6214=ORIENTED_EDGE('',*,*,#4764,.F.);
#6215=ORIENTED_EDGE('',*,*,#4765,.T.);
#6216=ORIENTED_EDGE('',*,*,#4766,.T.);
#6217=ORIENTED_EDGE('',*,*,#4765,.F.);
#6218=ORIENTED_EDGE('',*,*,#4767,.F.);
#6219=ORIENTED_EDGE('',*,*,#4768,.T.);
#6220=ORIENTED_EDGE('',*,*,#4769,.T.);
#6221=ORIENTED_EDGE('',*,*,#4768,.F.);
#6222=ORIENTED_EDGE('',*,*,#4767,.T.);
#6223=ORIENTED_EDGE('',*,*,#4764,.T.);
#6224=ORIENTED_EDGE('',*,*,#4769,.F.);
#6225=ORIENTED_EDGE('',*,*,#4766,.F.);
#6226=ORIENTED_EDGE('',*,*,#4770,.F.);
#6227=ORIENTED_EDGE('',*,*,#4771,.T.);
#6228=ORIENTED_EDGE('',*,*,#4772,.F.);
#6229=ORIENTED_EDGE('',*,*,#4773,.F.);
#6230=ORIENTED_EDGE('',*,*,#4774,.F.);
#6231=ORIENTED_EDGE('',*,*,#4775,.T.);
#6232=ORIENTED_EDGE('',*,*,#4776,.F.);
#6233=ORIENTED_EDGE('',*,*,#4777,.F.);
#6234=ORIENTED_EDGE('',*,*,#4775,.F.);
#6235=ORIENTED_EDGE('',*,*,#4778,.F.);
#6236=ORIENTED_EDGE('',*,*,#4771,.F.);
#6237=ORIENTED_EDGE('',*,*,#4779,.F.);
#6238=ORIENTED_EDGE('',*,*,#4773,.T.);
#6239=ORIENTED_EDGE('',*,*,#4780,.F.);
#6240=ORIENTED_EDGE('',*,*,#4781,.T.);
#6241=ORIENTED_EDGE('',*,*,#4782,.T.);
#6242=ORIENTED_EDGE('',*,*,#4781,.F.);
#6243=ORIENTED_EDGE('',*,*,#4778,.T.);
#6244=ORIENTED_EDGE('',*,*,#4774,.T.);
#6245=ORIENTED_EDGE('',*,*,#4779,.T.);
#6246=ORIENTED_EDGE('',*,*,#4772,.T.);
#6247=ORIENTED_EDGE('',*,*,#4770,.T.);
#6248=ORIENTED_EDGE('',*,*,#4783,.F.);
#6249=ORIENTED_EDGE('',*,*,#4784,.T.);
#6250=ORIENTED_EDGE('',*,*,#4785,.T.);
#6251=ORIENTED_EDGE('',*,*,#4784,.F.);
#6252=ORIENTED_EDGE('',*,*,#4776,.T.);
#6253=ORIENTED_EDGE('',*,*,#4777,.T.);
#6254=ORIENTED_EDGE('',*,*,#4783,.T.);
#6255=ORIENTED_EDGE('',*,*,#4780,.T.);
#6256=ORIENTED_EDGE('',*,*,#4785,.F.);
#6257=ORIENTED_EDGE('',*,*,#4782,.F.);
#6258=ORIENTED_EDGE('',*,*,#4786,.F.);
#6259=ORIENTED_EDGE('',*,*,#4787,.T.);
#6260=ORIENTED_EDGE('',*,*,#4788,.F.);
#6261=ORIENTED_EDGE('',*,*,#4787,.F.);
#6262=ORIENTED_EDGE('',*,*,#4786,.T.);
#6263=ORIENTED_EDGE('',*,*,#4789,.T.);
#6264=ORIENTED_EDGE('',*,*,#4790,.F.);
#6265=ORIENTED_EDGE('',*,*,#4791,.F.);
#6266=ORIENTED_EDGE('',*,*,#4792,.F.);
#6267=ORIENTED_EDGE('',*,*,#4789,.F.);
#6268=ORIENTED_EDGE('',*,*,#4793,.T.);
#6269=ORIENTED_EDGE('',*,*,#4791,.T.);
#6270=ORIENTED_EDGE('',*,*,#4793,.F.);
#6271=ORIENTED_EDGE('',*,*,#4792,.T.);
#6272=ORIENTED_EDGE('',*,*,#4794,.T.);
#6273=ORIENTED_EDGE('',*,*,#4795,.T.);
#6274=ORIENTED_EDGE('',*,*,#4794,.F.);
#6275=ORIENTED_EDGE('',*,*,#4796,.F.);
#6276=ORIENTED_EDGE('',*,*,#4797,.T.);
#6277=ORIENTED_EDGE('',*,*,#4790,.T.);
#6278=ORIENTED_EDGE('',*,*,#4797,.F.);
#6279=ORIENTED_EDGE('',*,*,#4796,.T.);
#6280=ORIENTED_EDGE('',*,*,#4788,.T.);
#6281=ORIENTED_EDGE('',*,*,#4795,.F.);
#6282=ORIENTED_EDGE('',*,*,#4798,.F.);
#6283=ORIENTED_EDGE('',*,*,#4799,.T.);
#6284=ORIENTED_EDGE('',*,*,#4800,.T.);
#6285=ORIENTED_EDGE('',*,*,#4799,.F.);
#6286=ORIENTED_EDGE('',*,*,#4801,.F.);
#6287=ORIENTED_EDGE('',*,*,#4802,.T.);
#6288=ORIENTED_EDGE('',*,*,#4803,.T.);
#6289=ORIENTED_EDGE('',*,*,#4802,.F.);
#6290=ORIENTED_EDGE('',*,*,#4801,.T.);
#6291=ORIENTED_EDGE('',*,*,#4798,.T.);
#6292=ORIENTED_EDGE('',*,*,#4803,.F.);
#6293=ORIENTED_EDGE('',*,*,#4800,.F.);
#6294=ORIENTED_EDGE('',*,*,#4804,.F.);
#6295=ORIENTED_EDGE('',*,*,#4805,.T.);
#6296=ORIENTED_EDGE('',*,*,#4806,.T.);
#6297=ORIENTED_EDGE('',*,*,#4805,.F.);
#6298=ORIENTED_EDGE('',*,*,#4807,.F.);
#6299=ORIENTED_EDGE('',*,*,#4808,.T.);
#6300=ORIENTED_EDGE('',*,*,#4809,.T.);
#6301=ORIENTED_EDGE('',*,*,#4808,.F.);
#6302=ORIENTED_EDGE('',*,*,#4807,.T.);
#6303=ORIENTED_EDGE('',*,*,#4804,.T.);
#6304=ORIENTED_EDGE('',*,*,#4809,.F.);
#6305=ORIENTED_EDGE('',*,*,#4806,.F.);
#6306=ORIENTED_EDGE('',*,*,#4810,.F.);
#6307=ORIENTED_EDGE('',*,*,#4811,.T.);
#6308=ORIENTED_EDGE('',*,*,#4812,.T.);
#6309=ORIENTED_EDGE('',*,*,#4811,.F.);
#6310=ORIENTED_EDGE('',*,*,#4813,.F.);
#6311=ORIENTED_EDGE('',*,*,#4814,.T.);
#6312=ORIENTED_EDGE('',*,*,#4815,.T.);
#6313=ORIENTED_EDGE('',*,*,#4814,.F.);
#6314=ORIENTED_EDGE('',*,*,#4813,.T.);
#6315=ORIENTED_EDGE('',*,*,#4810,.T.);
#6316=ORIENTED_EDGE('',*,*,#4815,.F.);
#6317=ORIENTED_EDGE('',*,*,#4812,.F.);
#6318=ORIENTED_EDGE('',*,*,#4816,.F.);
#6319=ORIENTED_EDGE('',*,*,#4817,.F.);
#6320=ORIENTED_EDGE('',*,*,#4818,.T.);
#6321=ORIENTED_EDGE('',*,*,#4816,.T.);
#6322=ORIENTED_EDGE('',*,*,#4818,.F.);
#6323=ORIENTED_EDGE('',*,*,#4819,.F.);
#6324=ORIENTED_EDGE('',*,*,#4820,.T.);
#6325=ORIENTED_EDGE('',*,*,#4817,.T.);
#6326=ORIENTED_EDGE('',*,*,#4820,.F.);
#6327=ORIENTED_EDGE('',*,*,#4821,.F.);
#6328=ORIENTED_EDGE('',*,*,#4822,.T.);
#6329=ORIENTED_EDGE('',*,*,#4819,.T.);
#6330=ORIENTED_EDGE('',*,*,#4822,.F.);
#6331=ORIENTED_EDGE('',*,*,#4821,.T.);
#6332=ORIENTED_EDGE('',*,*,#4823,.F.);
#6333=ORIENTED_EDGE('',*,*,#4824,.F.);
#6334=ORIENTED_EDGE('',*,*,#4825,.T.);
#6335=ORIENTED_EDGE('',*,*,#4823,.T.);
#6336=ORIENTED_EDGE('',*,*,#4825,.F.);
#6337=ORIENTED_EDGE('',*,*,#4826,.F.);
#6338=ORIENTED_EDGE('',*,*,#4827,.T.);
#6339=ORIENTED_EDGE('',*,*,#4824,.T.);
#6340=ORIENTED_EDGE('',*,*,#4827,.F.);
#6341=ORIENTED_EDGE('',*,*,#4828,.F.);
#6342=ORIENTED_EDGE('',*,*,#4829,.T.);
#6343=ORIENTED_EDGE('',*,*,#4826,.T.);
#6344=ORIENTED_EDGE('',*,*,#4829,.F.);
#6345=ORIENTED_EDGE('',*,*,#4828,.T.);
#6346=ORIENTED_EDGE('',*,*,#4830,.T.);
#6347=ORIENTED_EDGE('',*,*,#4831,.T.);
#6348=ORIENTED_EDGE('',*,*,#4832,.T.);
#6349=ORIENTED_EDGE('',*,*,#4833,.F.);
#6350=ORIENTED_EDGE('',*,*,#4834,.T.);
#6351=ORIENTED_EDGE('',*,*,#4835,.T.);
#6352=ORIENTED_EDGE('',*,*,#4836,.T.);
#6353=ORIENTED_EDGE('',*,*,#4831,.F.);
#6354=ORIENTED_EDGE('',*,*,#4837,.T.);
#6355=ORIENTED_EDGE('',*,*,#4838,.T.);
#6356=ORIENTED_EDGE('',*,*,#4839,.T.);
#6357=ORIENTED_EDGE('',*,*,#4835,.F.);
#6358=ORIENTED_EDGE('',*,*,#4840,.T.);
#6359=ORIENTED_EDGE('',*,*,#4841,.T.);
#6360=ORIENTED_EDGE('',*,*,#4842,.T.);
#6361=ORIENTED_EDGE('',*,*,#4838,.F.);
#6362=ORIENTED_EDGE('',*,*,#4843,.T.);
#6363=ORIENTED_EDGE('',*,*,#4844,.T.);
#6364=ORIENTED_EDGE('',*,*,#4845,.T.);
#6365=ORIENTED_EDGE('',*,*,#4841,.F.);
#6366=ORIENTED_EDGE('',*,*,#4846,.T.);
#6367=ORIENTED_EDGE('',*,*,#4833,.T.);
#6368=ORIENTED_EDGE('',*,*,#4847,.T.);
#6369=ORIENTED_EDGE('',*,*,#4844,.F.);
#6370=ORIENTED_EDGE('',*,*,#4846,.F.);
#6371=ORIENTED_EDGE('',*,*,#4843,.F.);
#6372=ORIENTED_EDGE('',*,*,#4840,.F.);
#6373=ORIENTED_EDGE('',*,*,#4837,.F.);
#6374=ORIENTED_EDGE('',*,*,#4834,.F.);
#6375=ORIENTED_EDGE('',*,*,#4830,.F.);
#6376=ORIENTED_EDGE('',*,*,#4847,.F.);
#6377=ORIENTED_EDGE('',*,*,#4832,.F.);
#6378=ORIENTED_EDGE('',*,*,#4836,.F.);
#6379=ORIENTED_EDGE('',*,*,#4839,.F.);
#6380=ORIENTED_EDGE('',*,*,#4842,.F.);
#6381=ORIENTED_EDGE('',*,*,#4845,.F.);
#6382=ORIENTED_EDGE('',*,*,#4848,.F.);
#6383=ORIENTED_EDGE('',*,*,#4849,.T.);
#6384=ORIENTED_EDGE('',*,*,#4850,.F.);
#6385=ORIENTED_EDGE('',*,*,#4849,.F.);
#6386=ORIENTED_EDGE('',*,*,#4851,.F.);
#6387=ORIENTED_EDGE('',*,*,#4852,.T.);
#6388=ORIENTED_EDGE('',*,*,#4853,.F.);
#6389=ORIENTED_EDGE('',*,*,#4854,.F.);
#6390=ORIENTED_EDGE('',*,*,#4855,.F.);
#6391=ORIENTED_EDGE('',*,*,#4854,.T.);
#6392=ORIENTED_EDGE('',*,*,#4856,.F.);
#6393=ORIENTED_EDGE('',*,*,#4857,.F.);
#6394=ORIENTED_EDGE('',*,*,#4858,.F.);
#6395=ORIENTED_EDGE('',*,*,#4857,.T.);
#6396=ORIENTED_EDGE('',*,*,#4859,.F.);
#6397=ORIENTED_EDGE('',*,*,#4860,.F.);
#6398=ORIENTED_EDGE('',*,*,#4861,.F.);
#6399=ORIENTED_EDGE('',*,*,#4860,.T.);
#6400=ORIENTED_EDGE('',*,*,#4862,.F.);
#6401=ORIENTED_EDGE('',*,*,#4852,.F.);
#6402=ORIENTED_EDGE('',*,*,#4863,.T.);
#6403=ORIENTED_EDGE('',*,*,#4864,.F.);
#6404=ORIENTED_EDGE('',*,*,#4865,.F.);
#6405=ORIENTED_EDGE('',*,*,#4866,.T.);
#6406=ORIENTED_EDGE('',*,*,#4867,.T.);
#6407=ORIENTED_EDGE('',*,*,#4868,.F.);
#6408=ORIENTED_EDGE('',*,*,#4869,.T.);
#6409=ORIENTED_EDGE('',*,*,#4866,.F.);
#6410=ORIENTED_EDGE('',*,*,#4848,.T.);
#6411=ORIENTED_EDGE('',*,*,#4858,.T.);
#6412=ORIENTED_EDGE('',*,*,#4861,.T.);
#6413=ORIENTED_EDGE('',*,*,#4851,.T.);
#6414=ORIENTED_EDGE('',*,*,#4855,.T.);
#6415=ORIENTED_EDGE('',*,*,#4870,.T.);
#6416=ORIENTED_EDGE('',*,*,#4869,.F.);
#6417=ORIENTED_EDGE('',*,*,#4871,.F.);
#6418=ORIENTED_EDGE('',*,*,#4872,.F.);
#6419=ORIENTED_EDGE('',*,*,#4863,.F.);
#6420=ORIENTED_EDGE('',*,*,#4867,.F.);
#6421=ORIENTED_EDGE('',*,*,#4865,.T.);
#6422=ORIENTED_EDGE('',*,*,#4873,.F.);
#6423=ORIENTED_EDGE('',*,*,#4874,.F.);
#6424=ORIENTED_EDGE('',*,*,#4871,.T.);
#6425=ORIENTED_EDGE('',*,*,#4868,.T.);
#6426=ORIENTED_EDGE('',*,*,#4874,.T.);
#6427=ORIENTED_EDGE('',*,*,#4875,.F.);
#6428=ORIENTED_EDGE('',*,*,#4876,.F.);
#6429=ORIENTED_EDGE('',*,*,#4877,.F.);
#6430=ORIENTED_EDGE('',*,*,#4870,.F.);
#6431=ORIENTED_EDGE('',*,*,#4878,.T.);
#6432=ORIENTED_EDGE('',*,*,#4876,.T.);
#6433=ORIENTED_EDGE('',*,*,#4878,.F.);
#6434=ORIENTED_EDGE('',*,*,#4877,.T.);
#6435=ORIENTED_EDGE('',*,*,#4879,.T.);
#6436=ORIENTED_EDGE('',*,*,#4880,.T.);
#6437=ORIENTED_EDGE('',*,*,#4879,.F.);
#6438=ORIENTED_EDGE('',*,*,#4872,.T.);
#6439=ORIENTED_EDGE('',*,*,#4875,.T.);
#6440=ORIENTED_EDGE('',*,*,#4873,.T.);
#6441=ORIENTED_EDGE('',*,*,#4864,.T.);
#6442=ORIENTED_EDGE('',*,*,#4850,.T.);
#6443=ORIENTED_EDGE('',*,*,#4859,.T.);
#6444=ORIENTED_EDGE('',*,*,#4856,.T.);
#6445=ORIENTED_EDGE('',*,*,#4853,.T.);
#6446=ORIENTED_EDGE('',*,*,#4862,.T.);
#6447=ORIENTED_EDGE('',*,*,#4880,.F.);
#6448=ORIENTED_EDGE('',*,*,#4881,.F.);
#6449=ORIENTED_EDGE('',*,*,#4882,.T.);
#6450=ORIENTED_EDGE('',*,*,#4883,.T.);
#6451=ORIENTED_EDGE('',*,*,#4882,.F.);
#6452=ORIENTED_EDGE('',*,*,#4884,.F.);
#6453=ORIENTED_EDGE('',*,*,#4885,.T.);
#6454=ORIENTED_EDGE('',*,*,#4886,.T.);
#6455=ORIENTED_EDGE('',*,*,#4885,.F.);
#6456=ORIENTED_EDGE('',*,*,#4884,.T.);
#6457=ORIENTED_EDGE('',*,*,#4881,.T.);
#6458=ORIENTED_EDGE('',*,*,#4886,.F.);
#6459=ORIENTED_EDGE('',*,*,#4883,.F.);
#6460=ORIENTED_EDGE('',*,*,#4887,.F.);
#6461=ORIENTED_EDGE('',*,*,#4888,.T.);
#6462=ORIENTED_EDGE('',*,*,#4889,.F.);
#6463=ORIENTED_EDGE('',*,*,#4890,.F.);
#6464=ORIENTED_EDGE('',*,*,#4891,.F.);
#6465=ORIENTED_EDGE('',*,*,#4892,.T.);
#6466=ORIENTED_EDGE('',*,*,#4893,.F.);
#6467=ORIENTED_EDGE('',*,*,#4894,.F.);
#6468=ORIENTED_EDGE('',*,*,#4892,.F.);
#6469=ORIENTED_EDGE('',*,*,#4895,.F.);
#6470=ORIENTED_EDGE('',*,*,#4888,.F.);
#6471=ORIENTED_EDGE('',*,*,#4896,.F.);
#6472=ORIENTED_EDGE('',*,*,#4890,.T.);
#6473=ORIENTED_EDGE('',*,*,#4897,.F.);
#6474=ORIENTED_EDGE('',*,*,#4898,.T.);
#6475=ORIENTED_EDGE('',*,*,#4899,.T.);
#6476=ORIENTED_EDGE('',*,*,#4898,.F.);
#6477=ORIENTED_EDGE('',*,*,#4895,.T.);
#6478=ORIENTED_EDGE('',*,*,#4891,.T.);
#6479=ORIENTED_EDGE('',*,*,#4896,.T.);
#6480=ORIENTED_EDGE('',*,*,#4889,.T.);
#6481=ORIENTED_EDGE('',*,*,#4887,.T.);
#6482=ORIENTED_EDGE('',*,*,#4900,.F.);
#6483=ORIENTED_EDGE('',*,*,#4901,.T.);
#6484=ORIENTED_EDGE('',*,*,#4902,.T.);
#6485=ORIENTED_EDGE('',*,*,#4901,.F.);
#6486=ORIENTED_EDGE('',*,*,#4893,.T.);
#6487=ORIENTED_EDGE('',*,*,#4894,.T.);
#6488=ORIENTED_EDGE('',*,*,#4900,.T.);
#6489=ORIENTED_EDGE('',*,*,#4897,.T.);
#6490=ORIENTED_EDGE('',*,*,#4902,.F.);
#6491=ORIENTED_EDGE('',*,*,#4899,.F.);
#6492=ORIENTED_EDGE('',*,*,#4903,.F.);
#6493=ORIENTED_EDGE('',*,*,#4904,.T.);
#6494=ORIENTED_EDGE('',*,*,#4905,.F.);
#6495=ORIENTED_EDGE('',*,*,#4904,.F.);
#6496=ORIENTED_EDGE('',*,*,#4903,.T.);
#6497=ORIENTED_EDGE('',*,*,#4906,.T.);
#6498=ORIENTED_EDGE('',*,*,#4907,.F.);
#6499=ORIENTED_EDGE('',*,*,#4908,.F.);
#6500=ORIENTED_EDGE('',*,*,#4909,.F.);
#6501=ORIENTED_EDGE('',*,*,#4906,.F.);
#6502=ORIENTED_EDGE('',*,*,#4910,.T.);
#6503=ORIENTED_EDGE('',*,*,#4908,.T.);
#6504=ORIENTED_EDGE('',*,*,#4910,.F.);
#6505=ORIENTED_EDGE('',*,*,#4909,.T.);
#6506=ORIENTED_EDGE('',*,*,#4911,.T.);
#6507=ORIENTED_EDGE('',*,*,#4912,.T.);
#6508=ORIENTED_EDGE('',*,*,#4911,.F.);
#6509=ORIENTED_EDGE('',*,*,#4913,.F.);
#6510=ORIENTED_EDGE('',*,*,#4914,.T.);
#6511=ORIENTED_EDGE('',*,*,#4907,.T.);
#6512=ORIENTED_EDGE('',*,*,#4914,.F.);
#6513=ORIENTED_EDGE('',*,*,#4913,.T.);
#6514=ORIENTED_EDGE('',*,*,#4905,.T.);
#6515=ORIENTED_EDGE('',*,*,#4912,.F.);
#6516=ORIENTED_EDGE('',*,*,#4915,.F.);
#6517=ORIENTED_EDGE('',*,*,#4916,.T.);
#6518=ORIENTED_EDGE('',*,*,#4917,.T.);
#6519=ORIENTED_EDGE('',*,*,#4916,.F.);
#6520=ORIENTED_EDGE('',*,*,#4918,.F.);
#6521=ORIENTED_EDGE('',*,*,#4919,.T.);
#6522=ORIENTED_EDGE('',*,*,#4920,.T.);
#6523=ORIENTED_EDGE('',*,*,#4919,.F.);
#6524=ORIENTED_EDGE('',*,*,#4918,.T.);
#6525=ORIENTED_EDGE('',*,*,#4915,.T.);
#6526=ORIENTED_EDGE('',*,*,#4920,.F.);
#6527=ORIENTED_EDGE('',*,*,#4917,.F.);
#6528=ORIENTED_EDGE('',*,*,#4921,.F.);
#6529=ORIENTED_EDGE('',*,*,#4922,.T.);
#6530=ORIENTED_EDGE('',*,*,#4923,.T.);
#6531=ORIENTED_EDGE('',*,*,#4922,.F.);
#6532=ORIENTED_EDGE('',*,*,#4924,.F.);
#6533=ORIENTED_EDGE('',*,*,#4925,.T.);
#6534=ORIENTED_EDGE('',*,*,#4926,.T.);
#6535=ORIENTED_EDGE('',*,*,#4925,.F.);
#6536=ORIENTED_EDGE('',*,*,#4924,.T.);
#6537=ORIENTED_EDGE('',*,*,#4921,.T.);
#6538=ORIENTED_EDGE('',*,*,#4926,.F.);
#6539=ORIENTED_EDGE('',*,*,#4923,.F.);
#6540=ORIENTED_EDGE('',*,*,#4927,.F.);
#6541=ORIENTED_EDGE('',*,*,#4928,.T.);
#6542=ORIENTED_EDGE('',*,*,#4929,.T.);
#6543=ORIENTED_EDGE('',*,*,#4928,.F.);
#6544=ORIENTED_EDGE('',*,*,#4930,.F.);
#6545=ORIENTED_EDGE('',*,*,#4931,.T.);
#6546=ORIENTED_EDGE('',*,*,#4932,.T.);
#6547=ORIENTED_EDGE('',*,*,#4931,.F.);
#6548=ORIENTED_EDGE('',*,*,#4930,.T.);
#6549=ORIENTED_EDGE('',*,*,#4927,.T.);
#6550=ORIENTED_EDGE('',*,*,#4932,.F.);
#6551=ORIENTED_EDGE('',*,*,#4929,.F.);
#6552=ORIENTED_EDGE('',*,*,#4933,.F.);
#6553=ORIENTED_EDGE('',*,*,#4934,.F.);
#6554=ORIENTED_EDGE('',*,*,#4935,.T.);
#6555=ORIENTED_EDGE('',*,*,#4936,.T.);
#6556=ORIENTED_EDGE('',*,*,#4937,.F.);
#6557=ORIENTED_EDGE('',*,*,#4938,.F.);
#6558=ORIENTED_EDGE('',*,*,#4939,.T.);
#6559=ORIENTED_EDGE('',*,*,#4940,.T.);
#6560=ORIENTED_EDGE('',*,*,#4935,.F.);
#6561=ORIENTED_EDGE('',*,*,#4941,.F.);
#6562=ORIENTED_EDGE('',*,*,#4942,.T.);
#6563=ORIENTED_EDGE('',*,*,#4943,.T.);
#6564=ORIENTED_EDGE('',*,*,#4939,.F.);
#6565=ORIENTED_EDGE('',*,*,#4944,.F.);
#6566=ORIENTED_EDGE('',*,*,#4945,.T.);
#6567=ORIENTED_EDGE('',*,*,#4946,.T.);
#6568=ORIENTED_EDGE('',*,*,#4942,.F.);
#6569=ORIENTED_EDGE('',*,*,#4947,.F.);
#6570=ORIENTED_EDGE('',*,*,#4948,.T.);
#6571=ORIENTED_EDGE('',*,*,#4949,.T.);
#6572=ORIENTED_EDGE('',*,*,#4945,.F.);
#6573=ORIENTED_EDGE('',*,*,#4950,.F.);
#6574=ORIENTED_EDGE('',*,*,#4937,.T.);
#6575=ORIENTED_EDGE('',*,*,#4951,.T.);
#6576=ORIENTED_EDGE('',*,*,#4948,.F.);
#6577=ORIENTED_EDGE('',*,*,#4951,.F.);
#6578=ORIENTED_EDGE('',*,*,#4936,.F.);
#6579=ORIENTED_EDGE('',*,*,#4940,.F.);
#6580=ORIENTED_EDGE('',*,*,#4943,.F.);
#6581=ORIENTED_EDGE('',*,*,#4946,.F.);
#6582=ORIENTED_EDGE('',*,*,#4949,.F.);
#6583=ORIENTED_EDGE('',*,*,#4952,.F.);
#6584=ORIENTED_EDGE('',*,*,#4934,.T.);
#6585=ORIENTED_EDGE('',*,*,#4950,.T.);
#6586=ORIENTED_EDGE('',*,*,#4947,.T.);
#6587=ORIENTED_EDGE('',*,*,#4944,.T.);
#6588=ORIENTED_EDGE('',*,*,#4941,.T.);
#6589=ORIENTED_EDGE('',*,*,#4938,.T.);
#6590=ORIENTED_EDGE('',*,*,#4953,.F.);
#6591=ORIENTED_EDGE('',*,*,#4954,.T.);
#6592=ORIENTED_EDGE('',*,*,#4952,.T.);
#6593=ORIENTED_EDGE('',*,*,#4954,.F.);
#6594=ORIENTED_EDGE('',*,*,#4933,.T.);
#6595=ORIENTED_EDGE('',*,*,#4955,.T.);
#6596=ORIENTED_EDGE('',*,*,#4953,.T.);
#6597=ORIENTED_EDGE('',*,*,#4955,.F.);
#6598=ORIENTED_EDGE('',*,*,#4956,.F.);
#6599=ORIENTED_EDGE('',*,*,#4957,.T.);
#6600=ORIENTED_EDGE('',*,*,#4958,.F.);
#6601=ORIENTED_EDGE('',*,*,#4957,.F.);
#6602=ORIENTED_EDGE('',*,*,#4959,.T.);
#6603=ORIENTED_EDGE('',*,*,#4960,.F.);
#6604=ORIENTED_EDGE('',*,*,#4961,.F.);
#6605=ORIENTED_EDGE('',*,*,#4962,.F.);
#6606=ORIENTED_EDGE('',*,*,#4963,.T.);
#6607=ORIENTED_EDGE('',*,*,#4964,.F.);
#6608=ORIENTED_EDGE('',*,*,#4965,.F.);
#6609=ORIENTED_EDGE('',*,*,#4966,.F.);
#6610=ORIENTED_EDGE('',*,*,#4961,.T.);
#6611=ORIENTED_EDGE('',*,*,#4967,.T.);
#6612=ORIENTED_EDGE('',*,*,#4968,.F.);
#6613=ORIENTED_EDGE('',*,*,#4969,.F.);
#6614=ORIENTED_EDGE('',*,*,#4965,.T.);
#6615=ORIENTED_EDGE('',*,*,#4970,.T.);
#6616=ORIENTED_EDGE('',*,*,#4971,.F.);
#6617=ORIENTED_EDGE('',*,*,#4972,.F.);
#6618=ORIENTED_EDGE('',*,*,#4971,.T.);
#6619=ORIENTED_EDGE('',*,*,#4973,.T.);
#6620=ORIENTED_EDGE('',*,*,#4968,.T.);
#6621=ORIENTED_EDGE('',*,*,#4974,.T.);
#6622=ORIENTED_EDGE('',*,*,#4958,.T.);
#6623=ORIENTED_EDGE('',*,*,#4975,.F.);
#6624=ORIENTED_EDGE('',*,*,#4976,.T.);
#6625=ORIENTED_EDGE('',*,*,#4977,.T.);
#6626=ORIENTED_EDGE('',*,*,#4978,.T.);
#6627=ORIENTED_EDGE('',*,*,#4979,.F.);
#6628=ORIENTED_EDGE('',*,*,#4980,.T.);
#6629=ORIENTED_EDGE('',*,*,#4981,.T.);
#6630=ORIENTED_EDGE('',*,*,#4982,.T.);
#6631=ORIENTED_EDGE('',*,*,#4983,.T.);
#6632=ORIENTED_EDGE('',*,*,#4984,.T.);
#6633=ORIENTED_EDGE('',*,*,#4981,.F.);
#6634=ORIENTED_EDGE('',*,*,#4985,.F.);
#6635=ORIENTED_EDGE('',*,*,#4986,.T.);
#6636=ORIENTED_EDGE('',*,*,#4987,.T.);
#6637=ORIENTED_EDGE('',*,*,#4977,.F.);
#6638=ORIENTED_EDGE('',*,*,#4988,.F.);
#6639=ORIENTED_EDGE('',*,*,#4986,.F.);
#6640=ORIENTED_EDGE('',*,*,#4989,.F.);
#6641=ORIENTED_EDGE('',*,*,#4983,.F.);
#6642=ORIENTED_EDGE('',*,*,#4990,.F.);
#6643=ORIENTED_EDGE('',*,*,#4956,.T.);
#6644=ORIENTED_EDGE('',*,*,#4991,.T.);
#6645=ORIENTED_EDGE('',*,*,#4966,.T.);
#6646=ORIENTED_EDGE('',*,*,#4972,.T.);
#6647=ORIENTED_EDGE('',*,*,#4974,.F.);
#6648=ORIENTED_EDGE('',*,*,#4967,.F.);
#6649=ORIENTED_EDGE('',*,*,#4960,.T.);
#6650=ORIENTED_EDGE('',*,*,#4992,.F.);
#6651=ORIENTED_EDGE('',*,*,#4982,.F.);
#6652=ORIENTED_EDGE('',*,*,#4984,.F.);
#6653=ORIENTED_EDGE('',*,*,#4989,.T.);
#6654=ORIENTED_EDGE('',*,*,#4988,.T.);
#6655=ORIENTED_EDGE('',*,*,#4976,.F.);
#6656=ORIENTED_EDGE('',*,*,#4979,.T.);
#6657=ORIENTED_EDGE('',*,*,#4992,.T.);
#6658=ORIENTED_EDGE('',*,*,#4959,.F.);
#6659=ORIENTED_EDGE('',*,*,#4993,.F.);
#6660=ORIENTED_EDGE('',*,*,#4993,.T.);
#6661=ORIENTED_EDGE('',*,*,#4962,.T.);
#6662=ORIENTED_EDGE('',*,*,#4969,.T.);
#6663=ORIENTED_EDGE('',*,*,#4973,.F.);
#6664=ORIENTED_EDGE('',*,*,#4970,.F.);
#6665=ORIENTED_EDGE('',*,*,#4964,.T.);
#6666=ORIENTED_EDGE('',*,*,#4994,.F.);
#6667=ORIENTED_EDGE('',*,*,#4978,.F.);
#6668=ORIENTED_EDGE('',*,*,#4987,.F.);
#6669=ORIENTED_EDGE('',*,*,#4990,.T.);
#6670=ORIENTED_EDGE('',*,*,#4985,.T.);
#6671=ORIENTED_EDGE('',*,*,#4980,.F.);
#6672=ORIENTED_EDGE('',*,*,#4975,.T.);
#6673=ORIENTED_EDGE('',*,*,#4994,.T.);
#6674=ORIENTED_EDGE('',*,*,#4963,.F.);
#6675=ORIENTED_EDGE('',*,*,#4991,.F.);
#6676=ORIENTED_EDGE('',*,*,#4995,.F.);
#6677=ORIENTED_EDGE('',*,*,#4996,.T.);
#6678=ORIENTED_EDGE('',*,*,#4997,.F.);
#6679=ORIENTED_EDGE('',*,*,#4996,.F.);
#6680=ORIENTED_EDGE('',*,*,#4998,.F.);
#6681=ORIENTED_EDGE('',*,*,#4999,.T.);
#6682=ORIENTED_EDGE('',*,*,#5000,.F.);
#6683=ORIENTED_EDGE('',*,*,#4999,.F.);
#6684=ORIENTED_EDGE('',*,*,#5001,.F.);
#6685=ORIENTED_EDGE('',*,*,#5002,.F.);
#6686=ORIENTED_EDGE('',*,*,#5003,.F.);
#6687=ORIENTED_EDGE('',*,*,#5004,.T.);
#6688=ORIENTED_EDGE('',*,*,#5001,.T.);
#6689=ORIENTED_EDGE('',*,*,#5005,.F.);
#6690=ORIENTED_EDGE('',*,*,#5006,.F.);
#6691=ORIENTED_EDGE('',*,*,#5007,.F.);
#6692=ORIENTED_EDGE('',*,*,#5004,.F.);
#6693=ORIENTED_EDGE('',*,*,#5008,.T.);
#6694=ORIENTED_EDGE('',*,*,#5009,.F.);
#6695=ORIENTED_EDGE('',*,*,#5005,.T.);
#6696=ORIENTED_EDGE('',*,*,#4995,.T.);
#6697=ORIENTED_EDGE('',*,*,#4998,.T.);
#6698=ORIENTED_EDGE('',*,*,#5003,.T.);
#6699=ORIENTED_EDGE('',*,*,#5010,.F.);
#6700=ORIENTED_EDGE('',*,*,#5011,.F.);
#6701=ORIENTED_EDGE('',*,*,#5008,.F.);
#6702=ORIENTED_EDGE('',*,*,#5006,.T.);
#6703=ORIENTED_EDGE('',*,*,#5009,.T.);
#6704=ORIENTED_EDGE('',*,*,#5011,.T.);
#6705=ORIENTED_EDGE('',*,*,#5012,.F.);
#6706=ORIENTED_EDGE('',*,*,#5007,.T.);
#6707=ORIENTED_EDGE('',*,*,#5012,.T.);
#6708=ORIENTED_EDGE('',*,*,#5010,.T.);
#6709=ORIENTED_EDGE('',*,*,#5002,.T.);
#6710=ORIENTED_EDGE('',*,*,#4997,.T.);
#6711=ORIENTED_EDGE('',*,*,#5000,.T.);
#6712=ORIENTED_EDGE('',*,*,#5013,.F.);
#6713=ORIENTED_EDGE('',*,*,#5014,.T.);
#6714=ORIENTED_EDGE('',*,*,#5015,.T.);
#6715=ORIENTED_EDGE('',*,*,#5014,.F.);
#6716=ORIENTED_EDGE('',*,*,#5016,.F.);
#6717=ORIENTED_EDGE('',*,*,#5017,.T.);
#6718=ORIENTED_EDGE('',*,*,#5018,.T.);
#6719=ORIENTED_EDGE('',*,*,#5017,.F.);
#6720=ORIENTED_EDGE('',*,*,#5016,.T.);
#6721=ORIENTED_EDGE('',*,*,#5013,.T.);
#6722=ORIENTED_EDGE('',*,*,#5018,.F.);
#6723=ORIENTED_EDGE('',*,*,#5015,.F.);
#6724=ORIENTED_EDGE('',*,*,#5019,.F.);
#6725=ORIENTED_EDGE('',*,*,#5020,.T.);
#6726=ORIENTED_EDGE('',*,*,#5021,.T.);
#6727=ORIENTED_EDGE('',*,*,#5020,.F.);
#6728=ORIENTED_EDGE('',*,*,#5022,.F.);
#6729=ORIENTED_EDGE('',*,*,#5023,.T.);
#6730=ORIENTED_EDGE('',*,*,#5024,.T.);
#6731=ORIENTED_EDGE('',*,*,#5023,.F.);
#6732=ORIENTED_EDGE('',*,*,#5022,.T.);
#6733=ORIENTED_EDGE('',*,*,#5019,.T.);
#6734=ORIENTED_EDGE('',*,*,#5024,.F.);
#6735=ORIENTED_EDGE('',*,*,#5021,.F.);
#6736=ORIENTED_EDGE('',*,*,#5025,.F.);
#6737=ORIENTED_EDGE('',*,*,#5026,.T.);
#6738=ORIENTED_EDGE('',*,*,#5027,.F.);
#6739=ORIENTED_EDGE('',*,*,#5026,.F.);
#6740=ORIENTED_EDGE('',*,*,#5028,.F.);
#6741=ORIENTED_EDGE('',*,*,#5029,.T.);
#6742=ORIENTED_EDGE('',*,*,#5030,.F.);
#6743=ORIENTED_EDGE('',*,*,#5029,.F.);
#6744=ORIENTED_EDGE('',*,*,#5031,.F.);
#6745=ORIENTED_EDGE('',*,*,#5032,.T.);
#6746=ORIENTED_EDGE('',*,*,#5033,.F.);
#6747=ORIENTED_EDGE('',*,*,#5032,.F.);
#6748=ORIENTED_EDGE('',*,*,#5034,.F.);
#6749=ORIENTED_EDGE('',*,*,#5035,.T.);
#6750=ORIENTED_EDGE('',*,*,#5036,.F.);
#6751=ORIENTED_EDGE('',*,*,#5035,.F.);
#6752=ORIENTED_EDGE('',*,*,#5037,.F.);
#6753=ORIENTED_EDGE('',*,*,#5038,.T.);
#6754=ORIENTED_EDGE('',*,*,#5039,.F.);
#6755=ORIENTED_EDGE('',*,*,#5038,.F.);
#6756=ORIENTED_EDGE('',*,*,#5040,.T.);
#6757=ORIENTED_EDGE('',*,*,#5041,.T.);
#6758=ORIENTED_EDGE('',*,*,#5042,.F.);
#6759=ORIENTED_EDGE('',*,*,#5043,.F.);
#6760=ORIENTED_EDGE('',*,*,#5044,.T.);
#6761=ORIENTED_EDGE('',*,*,#5043,.T.);
#6762=ORIENTED_EDGE('',*,*,#5045,.F.);
#6763=ORIENTED_EDGE('',*,*,#5046,.F.);
#6764=ORIENTED_EDGE('',*,*,#5047,.T.);
#6765=ORIENTED_EDGE('',*,*,#5046,.T.);
#6766=ORIENTED_EDGE('',*,*,#5048,.F.);
#6767=ORIENTED_EDGE('',*,*,#5049,.F.);
#6768=ORIENTED_EDGE('',*,*,#5050,.T.);
#6769=ORIENTED_EDGE('',*,*,#5049,.T.);
#6770=ORIENTED_EDGE('',*,*,#5051,.F.);
#6771=ORIENTED_EDGE('',*,*,#5041,.F.);
#6772=ORIENTED_EDGE('',*,*,#5051,.T.);
#6773=ORIENTED_EDGE('',*,*,#5048,.T.);
#6774=ORIENTED_EDGE('',*,*,#5045,.T.);
#6775=ORIENTED_EDGE('',*,*,#5042,.T.);
#6776=ORIENTED_EDGE('',*,*,#5027,.T.);
#6777=ORIENTED_EDGE('',*,*,#5030,.T.);
#6778=ORIENTED_EDGE('',*,*,#5033,.T.);
#6779=ORIENTED_EDGE('',*,*,#5036,.T.);
#6780=ORIENTED_EDGE('',*,*,#5039,.T.);
#6781=ORIENTED_EDGE('',*,*,#5050,.F.);
#6782=ORIENTED_EDGE('',*,*,#5040,.F.);
#6783=ORIENTED_EDGE('',*,*,#5044,.F.);
#6784=ORIENTED_EDGE('',*,*,#5047,.F.);
#6785=ORIENTED_EDGE('',*,*,#5025,.T.);
#6786=ORIENTED_EDGE('',*,*,#5028,.T.);
#6787=ORIENTED_EDGE('',*,*,#5031,.T.);
#6788=ORIENTED_EDGE('',*,*,#5034,.T.);
#6789=ORIENTED_EDGE('',*,*,#5037,.T.);
#6790=ORIENTED_EDGE('',*,*,#5052,.F.);
#6791=ORIENTED_EDGE('',*,*,#5053,.T.);
#6792=ORIENTED_EDGE('',*,*,#5054,.F.);
#6793=ORIENTED_EDGE('',*,*,#5053,.F.);
#6794=ORIENTED_EDGE('',*,*,#5052,.T.);
#6795=ORIENTED_EDGE('',*,*,#5055,.T.);
#6796=ORIENTED_EDGE('',*,*,#5056,.F.);
#6797=ORIENTED_EDGE('',*,*,#5057,.F.);
#6798=ORIENTED_EDGE('',*,*,#5058,.F.);
#6799=ORIENTED_EDGE('',*,*,#5055,.F.);
#6800=ORIENTED_EDGE('',*,*,#5059,.T.);
#6801=ORIENTED_EDGE('',*,*,#5057,.T.);
#6802=ORIENTED_EDGE('',*,*,#5059,.F.);
#6803=ORIENTED_EDGE('',*,*,#5058,.T.);
#6804=ORIENTED_EDGE('',*,*,#5060,.T.);
#6805=ORIENTED_EDGE('',*,*,#5061,.T.);
#6806=ORIENTED_EDGE('',*,*,#5060,.F.);
#6807=ORIENTED_EDGE('',*,*,#5062,.F.);
#6808=ORIENTED_EDGE('',*,*,#5063,.T.);
#6809=ORIENTED_EDGE('',*,*,#5056,.T.);
#6810=ORIENTED_EDGE('',*,*,#5063,.F.);
#6811=ORIENTED_EDGE('',*,*,#5062,.T.);
#6812=ORIENTED_EDGE('',*,*,#5054,.T.);
#6813=ORIENTED_EDGE('',*,*,#5061,.F.);
#6814=ORIENTED_EDGE('',*,*,#5064,.F.);
#6815=ORIENTED_EDGE('',*,*,#5065,.T.);
#6816=ORIENTED_EDGE('',*,*,#5066,.T.);
#6817=ORIENTED_EDGE('',*,*,#5065,.F.);
#6818=ORIENTED_EDGE('',*,*,#5067,.F.);
#6819=ORIENTED_EDGE('',*,*,#5068,.T.);
#6820=ORIENTED_EDGE('',*,*,#5069,.T.);
#6821=ORIENTED_EDGE('',*,*,#5068,.F.);
#6822=ORIENTED_EDGE('',*,*,#5067,.T.);
#6823=ORIENTED_EDGE('',*,*,#5064,.T.);
#6824=ORIENTED_EDGE('',*,*,#5069,.F.);
#6825=ORIENTED_EDGE('',*,*,#5066,.F.);
#6826=ORIENTED_EDGE('',*,*,#5070,.F.);
#6827=ORIENTED_EDGE('',*,*,#5071,.T.);
#6828=ORIENTED_EDGE('',*,*,#5072,.T.);
#6829=ORIENTED_EDGE('',*,*,#5071,.F.);
#6830=ORIENTED_EDGE('',*,*,#5073,.F.);
#6831=ORIENTED_EDGE('',*,*,#5074,.T.);
#6832=ORIENTED_EDGE('',*,*,#5075,.T.);
#6833=ORIENTED_EDGE('',*,*,#5074,.F.);
#6834=ORIENTED_EDGE('',*,*,#5073,.T.);
#6835=ORIENTED_EDGE('',*,*,#5070,.T.);
#6836=ORIENTED_EDGE('',*,*,#5075,.F.);
#6837=ORIENTED_EDGE('',*,*,#5072,.F.);
#6838=ORIENTED_EDGE('',*,*,#5076,.F.);
#6839=ORIENTED_EDGE('',*,*,#5077,.T.);
#6840=ORIENTED_EDGE('',*,*,#5078,.T.);
#6841=ORIENTED_EDGE('',*,*,#5077,.F.);
#6842=ORIENTED_EDGE('',*,*,#5079,.F.);
#6843=ORIENTED_EDGE('',*,*,#5080,.T.);
#6844=ORIENTED_EDGE('',*,*,#5081,.T.);
#6845=ORIENTED_EDGE('',*,*,#5080,.F.);
#6846=ORIENTED_EDGE('',*,*,#5079,.T.);
#6847=ORIENTED_EDGE('',*,*,#5076,.T.);
#6848=ORIENTED_EDGE('',*,*,#5081,.F.);
#6849=ORIENTED_EDGE('',*,*,#5078,.F.);
#6850=ORIENTED_EDGE('',*,*,#5082,.F.);
#6851=ORIENTED_EDGE('',*,*,#5083,.T.);
#6852=ORIENTED_EDGE('',*,*,#5084,.F.);
#6853=ORIENTED_EDGE('',*,*,#5085,.F.);
#6854=ORIENTED_EDGE('',*,*,#5086,.T.);
#6855=ORIENTED_EDGE('',*,*,#5087,.F.);
#6856=ORIENTED_EDGE('',*,*,#5086,.F.);
#6857=ORIENTED_EDGE('',*,*,#5088,.F.);
#6858=ORIENTED_EDGE('',*,*,#5089,.F.);
#6859=ORIENTED_EDGE('',*,*,#5083,.F.);
#6860=ORIENTED_EDGE('',*,*,#5090,.F.);
#6861=ORIENTED_EDGE('',*,*,#5091,.T.);
#6862=ORIENTED_EDGE('',*,*,#5092,.F.);
#6863=ORIENTED_EDGE('',*,*,#5093,.F.);
#6864=ORIENTED_EDGE('',*,*,#5094,.T.);
#6865=ORIENTED_EDGE('',*,*,#5095,.F.);
#6866=ORIENTED_EDGE('',*,*,#5094,.F.);
#6867=ORIENTED_EDGE('',*,*,#5096,.F.);
#6868=ORIENTED_EDGE('',*,*,#5097,.F.);
#6869=ORIENTED_EDGE('',*,*,#5091,.F.);
#6870=ORIENTED_EDGE('',*,*,#5098,.F.);
#6871=ORIENTED_EDGE('',*,*,#5099,.T.);
#6872=ORIENTED_EDGE('',*,*,#5100,.F.);
#6873=ORIENTED_EDGE('',*,*,#5101,.F.);
#6874=ORIENTED_EDGE('',*,*,#5102,.T.);
#6875=ORIENTED_EDGE('',*,*,#5103,.F.);
#6876=ORIENTED_EDGE('',*,*,#5102,.F.);
#6877=ORIENTED_EDGE('',*,*,#5104,.F.);
#6878=ORIENTED_EDGE('',*,*,#5105,.F.);
#6879=ORIENTED_EDGE('',*,*,#5099,.F.);
#6880=ORIENTED_EDGE('',*,*,#5106,.F.);
#6881=ORIENTED_EDGE('',*,*,#5107,.T.);
#6882=ORIENTED_EDGE('',*,*,#5108,.F.);
#6883=ORIENTED_EDGE('',*,*,#5109,.F.);
#6884=ORIENTED_EDGE('',*,*,#5110,.T.);
#6885=ORIENTED_EDGE('',*,*,#5111,.F.);
#6886=ORIENTED_EDGE('',*,*,#5110,.F.);
#6887=ORIENTED_EDGE('',*,*,#5112,.F.);
#6888=ORIENTED_EDGE('',*,*,#5113,.F.);
#6889=ORIENTED_EDGE('',*,*,#5107,.F.);
#6890=ORIENTED_EDGE('',*,*,#5084,.T.);
#6891=ORIENTED_EDGE('',*,*,#5082,.T.);
#6892=ORIENTED_EDGE('',*,*,#5089,.T.);
#6893=ORIENTED_EDGE('',*,*,#5114,.T.);
#6894=ORIENTED_EDGE('',*,*,#5100,.T.);
#6895=ORIENTED_EDGE('',*,*,#5098,.T.);
#6896=ORIENTED_EDGE('',*,*,#5105,.T.);
#6897=ORIENTED_EDGE('',*,*,#5115,.T.);
#6898=ORIENTED_EDGE('',*,*,#5116,.F.);
#6899=ORIENTED_EDGE('',*,*,#5117,.T.);
#6900=ORIENTED_EDGE('',*,*,#5118,.F.);
#6901=ORIENTED_EDGE('',*,*,#5119,.T.);
#6902=ORIENTED_EDGE('',*,*,#5092,.T.);
#6903=ORIENTED_EDGE('',*,*,#5090,.T.);
#6904=ORIENTED_EDGE('',*,*,#5097,.T.);
#6905=ORIENTED_EDGE('',*,*,#5120,.T.);
#6906=ORIENTED_EDGE('',*,*,#5108,.T.);
#6907=ORIENTED_EDGE('',*,*,#5106,.T.);
#6908=ORIENTED_EDGE('',*,*,#5113,.T.);
#6909=ORIENTED_EDGE('',*,*,#5121,.T.);
#6910=ORIENTED_EDGE('',*,*,#5122,.F.);
#6911=ORIENTED_EDGE('',*,*,#5123,.F.);
#6912=ORIENTED_EDGE('',*,*,#5124,.F.);
#6913=ORIENTED_EDGE('',*,*,#5125,.T.);
#6914=ORIENTED_EDGE('',*,*,#5116,.T.);
#6915=ORIENTED_EDGE('',*,*,#5126,.T.);
#6916=ORIENTED_EDGE('',*,*,#5127,.T.);
#6917=ORIENTED_EDGE('',*,*,#5128,.T.);
#6918=ORIENTED_EDGE('',*,*,#5129,.T.);
#6919=ORIENTED_EDGE('',*,*,#5130,.T.);
#6920=ORIENTED_EDGE('',*,*,#5124,.T.);
#6921=ORIENTED_EDGE('',*,*,#5131,.T.);
#6922=ORIENTED_EDGE('',*,*,#5132,.T.);
#6923=ORIENTED_EDGE('',*,*,#5133,.T.);
#6924=ORIENTED_EDGE('',*,*,#5134,.T.);
#6925=ORIENTED_EDGE('',*,*,#5135,.T.);
#6926=ORIENTED_EDGE('',*,*,#5088,.T.);
#6927=ORIENTED_EDGE('',*,*,#5085,.T.);
#6928=ORIENTED_EDGE('',*,*,#5119,.F.);
#6929=ORIENTED_EDGE('',*,*,#5136,.F.);
#6930=ORIENTED_EDGE('',*,*,#5137,.F.);
#6931=ORIENTED_EDGE('',*,*,#5126,.F.);
#6932=ORIENTED_EDGE('',*,*,#5115,.F.);
#6933=ORIENTED_EDGE('',*,*,#5104,.T.);
#6934=ORIENTED_EDGE('',*,*,#5101,.T.);
#6935=ORIENTED_EDGE('',*,*,#5114,.F.);
#6936=ORIENTED_EDGE('',*,*,#5137,.T.);
#6937=ORIENTED_EDGE('',*,*,#5138,.F.);
#6938=ORIENTED_EDGE('',*,*,#5139,.F.);
#6939=ORIENTED_EDGE('',*,*,#5127,.F.);
#6940=ORIENTED_EDGE('',*,*,#5139,.T.);
#6941=ORIENTED_EDGE('',*,*,#5140,.F.);
#6942=ORIENTED_EDGE('',*,*,#5141,.F.);
#6943=ORIENTED_EDGE('',*,*,#5128,.F.);
#6944=ORIENTED_EDGE('',*,*,#5087,.T.);
#6945=ORIENTED_EDGE('',*,*,#5095,.T.);
#6946=ORIENTED_EDGE('',*,*,#5103,.T.);
#6947=ORIENTED_EDGE('',*,*,#5111,.T.);
#6948=ORIENTED_EDGE('',*,*,#5141,.T.);
#6949=ORIENTED_EDGE('',*,*,#5142,.F.);
#6950=ORIENTED_EDGE('',*,*,#5143,.F.);
#6951=ORIENTED_EDGE('',*,*,#5129,.F.);
#6952=ORIENTED_EDGE('',*,*,#5096,.T.);
#6953=ORIENTED_EDGE('',*,*,#5093,.T.);
#6954=ORIENTED_EDGE('',*,*,#5125,.F.);
#6955=ORIENTED_EDGE('',*,*,#5130,.F.);
#6956=ORIENTED_EDGE('',*,*,#5143,.T.);
#6957=ORIENTED_EDGE('',*,*,#5144,.F.);
#6958=ORIENTED_EDGE('',*,*,#5121,.F.);
#6959=ORIENTED_EDGE('',*,*,#5112,.T.);
#6960=ORIENTED_EDGE('',*,*,#5109,.T.);
#6961=ORIENTED_EDGE('',*,*,#5120,.F.);
#6962=ORIENTED_EDGE('',*,*,#5123,.T.);
#6963=ORIENTED_EDGE('',*,*,#5145,.F.);
#6964=ORIENTED_EDGE('',*,*,#5146,.F.);
#6965=ORIENTED_EDGE('',*,*,#5131,.F.);
#6966=ORIENTED_EDGE('',*,*,#5146,.T.);
#6967=ORIENTED_EDGE('',*,*,#5147,.F.);
#6968=ORIENTED_EDGE('',*,*,#5148,.F.);
#6969=ORIENTED_EDGE('',*,*,#5132,.F.);
#6970=ORIENTED_EDGE('',*,*,#5148,.T.);
#6971=ORIENTED_EDGE('',*,*,#5149,.F.);
#6972=ORIENTED_EDGE('',*,*,#5150,.F.);
#6973=ORIENTED_EDGE('',*,*,#5133,.F.);
#6974=ORIENTED_EDGE('',*,*,#5150,.T.);
#6975=ORIENTED_EDGE('',*,*,#5151,.F.);
#6976=ORIENTED_EDGE('',*,*,#5152,.F.);
#6977=ORIENTED_EDGE('',*,*,#5134,.F.);
#6978=ORIENTED_EDGE('',*,*,#5152,.T.);
#6979=ORIENTED_EDGE('',*,*,#5153,.F.);
#6980=ORIENTED_EDGE('',*,*,#5117,.F.);
#6981=ORIENTED_EDGE('',*,*,#5135,.F.);
#6982=ORIENTED_EDGE('',*,*,#5118,.T.);
#6983=ORIENTED_EDGE('',*,*,#5153,.T.);
#6984=ORIENTED_EDGE('',*,*,#5151,.T.);
#6985=ORIENTED_EDGE('',*,*,#5149,.T.);
#6986=ORIENTED_EDGE('',*,*,#5147,.T.);
#6987=ORIENTED_EDGE('',*,*,#5145,.T.);
#6988=ORIENTED_EDGE('',*,*,#5122,.T.);
#6989=ORIENTED_EDGE('',*,*,#5144,.T.);
#6990=ORIENTED_EDGE('',*,*,#5142,.T.);
#6991=ORIENTED_EDGE('',*,*,#5140,.T.);
#6992=ORIENTED_EDGE('',*,*,#5138,.T.);
#6993=ORIENTED_EDGE('',*,*,#5136,.T.);
#6994=ORIENTED_EDGE('',*,*,#5154,.T.);
#6995=ORIENTED_EDGE('',*,*,#5155,.T.);
#6996=ORIENTED_EDGE('',*,*,#5156,.F.);
#6997=ORIENTED_EDGE('',*,*,#5157,.F.);
#6998=ORIENTED_EDGE('',*,*,#5158,.T.);
#6999=ORIENTED_EDGE('',*,*,#5157,.T.);
#7000=ORIENTED_EDGE('',*,*,#5159,.F.);
#7001=ORIENTED_EDGE('',*,*,#5160,.F.);
#7002=ORIENTED_EDGE('',*,*,#5161,.T.);
#7003=ORIENTED_EDGE('',*,*,#5160,.T.);
#7004=ORIENTED_EDGE('',*,*,#5162,.F.);
#7005=ORIENTED_EDGE('',*,*,#5163,.F.);
#7006=ORIENTED_EDGE('',*,*,#5164,.T.);
#7007=ORIENTED_EDGE('',*,*,#5163,.T.);
#7008=ORIENTED_EDGE('',*,*,#5165,.F.);
#7009=ORIENTED_EDGE('',*,*,#5166,.F.);
#7010=ORIENTED_EDGE('',*,*,#5167,.T.);
#7011=ORIENTED_EDGE('',*,*,#5166,.T.);
#7012=ORIENTED_EDGE('',*,*,#5168,.F.);
#7013=ORIENTED_EDGE('',*,*,#5169,.F.);
#7014=ORIENTED_EDGE('',*,*,#5170,.T.);
#7015=ORIENTED_EDGE('',*,*,#5169,.T.);
#7016=ORIENTED_EDGE('',*,*,#5171,.F.);
#7017=ORIENTED_EDGE('',*,*,#5172,.F.);
#7018=ORIENTED_EDGE('',*,*,#5173,.T.);
#7019=ORIENTED_EDGE('',*,*,#5172,.T.);
#7020=ORIENTED_EDGE('',*,*,#5174,.F.);
#7021=ORIENTED_EDGE('',*,*,#5175,.F.);
#7022=ORIENTED_EDGE('',*,*,#5176,.T.);
#7023=ORIENTED_EDGE('',*,*,#5175,.T.);
#7024=ORIENTED_EDGE('',*,*,#5177,.F.);
#7025=ORIENTED_EDGE('',*,*,#5155,.F.);
#7026=ORIENTED_EDGE('',*,*,#5177,.T.);
#7027=ORIENTED_EDGE('',*,*,#5174,.T.);
#7028=ORIENTED_EDGE('',*,*,#5171,.T.);
#7029=ORIENTED_EDGE('',*,*,#5168,.T.);
#7030=ORIENTED_EDGE('',*,*,#5165,.T.);
#7031=ORIENTED_EDGE('',*,*,#5162,.T.);
#7032=ORIENTED_EDGE('',*,*,#5159,.T.);
#7033=ORIENTED_EDGE('',*,*,#5156,.T.);
#7034=ORIENTED_EDGE('',*,*,#5176,.F.);
#7035=ORIENTED_EDGE('',*,*,#5154,.F.);
#7036=ORIENTED_EDGE('',*,*,#5158,.F.);
#7037=ORIENTED_EDGE('',*,*,#5161,.F.);
#7038=ORIENTED_EDGE('',*,*,#5164,.F.);
#7039=ORIENTED_EDGE('',*,*,#5167,.F.);
#7040=ORIENTED_EDGE('',*,*,#5170,.F.);
#7041=ORIENTED_EDGE('',*,*,#5173,.F.);
#7042=ORIENTED_EDGE('',*,*,#5178,.F.);
#7043=ORIENTED_EDGE('',*,*,#5179,.T.);
#7044=ORIENTED_EDGE('',*,*,#5180,.F.);
#7045=ORIENTED_EDGE('',*,*,#5181,.F.);
#7046=ORIENTED_EDGE('',*,*,#5182,.F.);
#7047=ORIENTED_EDGE('',*,*,#5181,.T.);
#7048=ORIENTED_EDGE('',*,*,#5183,.F.);
#7049=ORIENTED_EDGE('',*,*,#5184,.F.);
#7050=ORIENTED_EDGE('',*,*,#5185,.F.);
#7051=ORIENTED_EDGE('',*,*,#5184,.T.);
#7052=ORIENTED_EDGE('',*,*,#5186,.F.);
#7053=ORIENTED_EDGE('',*,*,#5187,.F.);
#7054=ORIENTED_EDGE('',*,*,#5188,.F.);
#7055=ORIENTED_EDGE('',*,*,#5187,.T.);
#7056=ORIENTED_EDGE('',*,*,#5189,.F.);
#7057=ORIENTED_EDGE('',*,*,#5190,.F.);
#7058=ORIENTED_EDGE('',*,*,#5191,.F.);
#7059=ORIENTED_EDGE('',*,*,#5190,.T.);
#7060=ORIENTED_EDGE('',*,*,#5192,.F.);
#7061=ORIENTED_EDGE('',*,*,#5193,.F.);
#7062=ORIENTED_EDGE('',*,*,#5194,.F.);
#7063=ORIENTED_EDGE('',*,*,#5193,.T.);
#7064=ORIENTED_EDGE('',*,*,#5195,.F.);
#7065=ORIENTED_EDGE('',*,*,#5196,.F.);
#7066=ORIENTED_EDGE('',*,*,#5197,.F.);
#7067=ORIENTED_EDGE('',*,*,#5196,.T.);
#7068=ORIENTED_EDGE('',*,*,#5198,.F.);
#7069=ORIENTED_EDGE('',*,*,#5199,.F.);
#7070=ORIENTED_EDGE('',*,*,#5200,.F.);
#7071=ORIENTED_EDGE('',*,*,#5199,.T.);
#7072=ORIENTED_EDGE('',*,*,#5201,.F.);
#7073=ORIENTED_EDGE('',*,*,#5179,.F.);
#7074=ORIENTED_EDGE('',*,*,#5200,.T.);
#7075=ORIENTED_EDGE('',*,*,#5178,.T.);
#7076=ORIENTED_EDGE('',*,*,#5182,.T.);
#7077=ORIENTED_EDGE('',*,*,#5185,.T.);
#7078=ORIENTED_EDGE('',*,*,#5188,.T.);
#7079=ORIENTED_EDGE('',*,*,#5191,.T.);
#7080=ORIENTED_EDGE('',*,*,#5194,.T.);
#7081=ORIENTED_EDGE('',*,*,#5197,.T.);
#7082=ORIENTED_EDGE('',*,*,#5201,.T.);
#7083=ORIENTED_EDGE('',*,*,#5198,.T.);
#7084=ORIENTED_EDGE('',*,*,#5195,.T.);
#7085=ORIENTED_EDGE('',*,*,#5192,.T.);
#7086=ORIENTED_EDGE('',*,*,#5189,.T.);
#7087=ORIENTED_EDGE('',*,*,#5186,.T.);
#7088=ORIENTED_EDGE('',*,*,#5183,.T.);
#7089=ORIENTED_EDGE('',*,*,#5180,.T.);
#7090=ORIENTED_EDGE('',*,*,#5202,.T.);
#7091=ORIENTED_EDGE('',*,*,#5203,.T.);
#7092=ORIENTED_EDGE('',*,*,#5204,.T.);
#7093=ORIENTED_EDGE('',*,*,#5205,.F.);
#7094=ORIENTED_EDGE('',*,*,#5206,.T.);
#7095=ORIENTED_EDGE('',*,*,#5207,.T.);
#7096=ORIENTED_EDGE('',*,*,#5208,.T.);
#7097=ORIENTED_EDGE('',*,*,#5203,.F.);
#7098=ORIENTED_EDGE('',*,*,#5209,.T.);
#7099=ORIENTED_EDGE('',*,*,#5210,.T.);
#7100=ORIENTED_EDGE('',*,*,#5211,.T.);
#7101=ORIENTED_EDGE('',*,*,#5207,.F.);
#7102=ORIENTED_EDGE('',*,*,#5212,.T.);
#7103=ORIENTED_EDGE('',*,*,#5213,.T.);
#7104=ORIENTED_EDGE('',*,*,#5214,.T.);
#7105=ORIENTED_EDGE('',*,*,#5210,.F.);
#7106=ORIENTED_EDGE('',*,*,#5215,.T.);
#7107=ORIENTED_EDGE('',*,*,#5216,.T.);
#7108=ORIENTED_EDGE('',*,*,#5217,.T.);
#7109=ORIENTED_EDGE('',*,*,#5213,.F.);
#7110=ORIENTED_EDGE('',*,*,#5218,.T.);
#7111=ORIENTED_EDGE('',*,*,#5205,.T.);
#7112=ORIENTED_EDGE('',*,*,#5219,.T.);
#7113=ORIENTED_EDGE('',*,*,#5216,.F.);
#7114=ORIENTED_EDGE('',*,*,#5218,.F.);
#7115=ORIENTED_EDGE('',*,*,#5215,.F.);
#7116=ORIENTED_EDGE('',*,*,#5212,.F.);
#7117=ORIENTED_EDGE('',*,*,#5209,.F.);
#7118=ORIENTED_EDGE('',*,*,#5206,.F.);
#7119=ORIENTED_EDGE('',*,*,#5202,.F.);
#7120=ORIENTED_EDGE('',*,*,#5219,.F.);
#7121=ORIENTED_EDGE('',*,*,#5204,.F.);
#7122=ORIENTED_EDGE('',*,*,#5208,.F.);
#7123=ORIENTED_EDGE('',*,*,#5211,.F.);
#7124=ORIENTED_EDGE('',*,*,#5214,.F.);
#7125=ORIENTED_EDGE('',*,*,#5217,.F.);
#7126=ORIENTED_EDGE('',*,*,#5220,.F.);
#7127=ORIENTED_EDGE('',*,*,#5221,.F.);
#7128=ORIENTED_EDGE('',*,*,#5222,.F.);
#7129=ORIENTED_EDGE('',*,*,#5223,.T.);
#7130=ORIENTED_EDGE('',*,*,#5221,.T.);
#7131=ORIENTED_EDGE('',*,*,#5223,.F.);
#7132=ORIENTED_EDGE('',*,*,#5224,.F.);
#7133=ORIENTED_EDGE('',*,*,#5225,.T.);
#7134=ORIENTED_EDGE('',*,*,#5222,.T.);
#7135=ORIENTED_EDGE('',*,*,#5225,.F.);
#7136=ORIENTED_EDGE('',*,*,#5226,.F.);
#7137=ORIENTED_EDGE('',*,*,#5227,.T.);
#7138=ORIENTED_EDGE('',*,*,#5224,.T.);
#7139=ORIENTED_EDGE('',*,*,#5227,.F.);
#7140=ORIENTED_EDGE('',*,*,#5226,.T.);
#7141=ORIENTED_EDGE('',*,*,#5228,.F.);
#7142=ORIENTED_EDGE('',*,*,#5229,.F.);
#7143=ORIENTED_EDGE('',*,*,#5230,.T.);
#7144=ORIENTED_EDGE('',*,*,#5228,.T.);
#7145=ORIENTED_EDGE('',*,*,#5230,.F.);
#7146=ORIENTED_EDGE('',*,*,#5220,.T.);
#7147=ORIENTED_EDGE('',*,*,#5231,.T.);
#7148=ORIENTED_EDGE('',*,*,#5229,.T.);
#7149=ORIENTED_EDGE('',*,*,#5231,.F.);
#7150=ORIENTED_EDGE('',*,*,#5232,.T.);
#7151=ORIENTED_EDGE('',*,*,#5233,.T.);
#7152=ORIENTED_EDGE('',*,*,#5234,.T.);
#7153=ORIENTED_EDGE('',*,*,#5235,.F.);
#7154=ORIENTED_EDGE('',*,*,#5236,.T.);
#7155=ORIENTED_EDGE('',*,*,#5237,.T.);
#7156=ORIENTED_EDGE('',*,*,#5238,.T.);
#7157=ORIENTED_EDGE('',*,*,#5233,.F.);
#7158=ORIENTED_EDGE('',*,*,#5239,.T.);
#7159=ORIENTED_EDGE('',*,*,#5240,.T.);
#7160=ORIENTED_EDGE('',*,*,#5241,.T.);
#7161=ORIENTED_EDGE('',*,*,#5237,.F.);
#7162=ORIENTED_EDGE('',*,*,#5242,.T.);
#7163=ORIENTED_EDGE('',*,*,#5243,.T.);
#7164=ORIENTED_EDGE('',*,*,#5244,.T.);
#7165=ORIENTED_EDGE('',*,*,#5240,.F.);
#7166=ORIENTED_EDGE('',*,*,#5245,.T.);
#7167=ORIENTED_EDGE('',*,*,#5246,.T.);
#7168=ORIENTED_EDGE('',*,*,#5247,.T.);
#7169=ORIENTED_EDGE('',*,*,#5243,.F.);
#7170=ORIENTED_EDGE('',*,*,#5248,.T.);
#7171=ORIENTED_EDGE('',*,*,#5235,.T.);
#7172=ORIENTED_EDGE('',*,*,#5249,.T.);
#7173=ORIENTED_EDGE('',*,*,#5246,.F.);
#7174=ORIENTED_EDGE('',*,*,#5248,.F.);
#7175=ORIENTED_EDGE('',*,*,#5245,.F.);
#7176=ORIENTED_EDGE('',*,*,#5242,.F.);
#7177=ORIENTED_EDGE('',*,*,#5239,.F.);
#7178=ORIENTED_EDGE('',*,*,#5236,.F.);
#7179=ORIENTED_EDGE('',*,*,#5232,.F.);
#7180=ORIENTED_EDGE('',*,*,#5249,.F.);
#7181=ORIENTED_EDGE('',*,*,#5234,.F.);
#7182=ORIENTED_EDGE('',*,*,#5238,.F.);
#7183=ORIENTED_EDGE('',*,*,#5241,.F.);
#7184=ORIENTED_EDGE('',*,*,#5244,.F.);
#7185=ORIENTED_EDGE('',*,*,#5247,.F.);
#7186=ORIENTED_EDGE('',*,*,#5250,.F.);
#7187=ORIENTED_EDGE('',*,*,#5251,.F.);
#7188=ORIENTED_EDGE('',*,*,#5252,.F.);
#7189=ORIENTED_EDGE('',*,*,#5253,.T.);
#7190=ORIENTED_EDGE('',*,*,#5251,.T.);
#7191=ORIENTED_EDGE('',*,*,#5253,.F.);
#7192=ORIENTED_EDGE('',*,*,#5254,.F.);
#7193=ORIENTED_EDGE('',*,*,#5255,.T.);
#7194=ORIENTED_EDGE('',*,*,#5252,.T.);
#7195=ORIENTED_EDGE('',*,*,#5255,.F.);
#7196=ORIENTED_EDGE('',*,*,#5256,.F.);
#7197=ORIENTED_EDGE('',*,*,#5257,.T.);
#7198=ORIENTED_EDGE('',*,*,#5254,.T.);
#7199=ORIENTED_EDGE('',*,*,#5257,.F.);
#7200=ORIENTED_EDGE('',*,*,#5256,.T.);
#7201=ORIENTED_EDGE('',*,*,#5258,.F.);
#7202=ORIENTED_EDGE('',*,*,#5259,.F.);
#7203=ORIENTED_EDGE('',*,*,#5260,.T.);
#7204=ORIENTED_EDGE('',*,*,#5258,.T.);
#7205=ORIENTED_EDGE('',*,*,#5260,.F.);
#7206=ORIENTED_EDGE('',*,*,#5250,.T.);
#7207=ORIENTED_EDGE('',*,*,#5261,.T.);
#7208=ORIENTED_EDGE('',*,*,#5259,.T.);
#7209=ORIENTED_EDGE('',*,*,#5261,.F.);
#7210=CYLINDRICAL_SURFACE('',#8387,0.21);
#7211=CYLINDRICAL_SURFACE('',#8390,0.21);
#7212=CYLINDRICAL_SURFACE('',#8393,0.21);
#7213=CYLINDRICAL_SURFACE('',#8396,0.21);
#7214=CYLINDRICAL_SURFACE('',#8399,0.21);
#7215=CYLINDRICAL_SURFACE('',#8402,0.21);
#7216=CYLINDRICAL_SURFACE('',#8405,0.21);
#7217=CYLINDRICAL_SURFACE('',#8408,0.21);
#7218=CYLINDRICAL_SURFACE('',#8411,0.164999999999999);
#7219=CYLINDRICAL_SURFACE('',#8414,0.164999999999999);
#7220=CYLINDRICAL_SURFACE('',#8417,0.165);
#7221=CYLINDRICAL_SURFACE('',#8420,0.165);
#7222=CYLINDRICAL_SURFACE('',#8444,0.25);
#7223=CYLINDRICAL_SURFACE('',#8445,0.165);
#7224=CYLINDRICAL_SURFACE('',#8449,0.165);
#7225=CYLINDRICAL_SURFACE('',#8453,0.165);
#7226=CYLINDRICAL_SURFACE('',#8457,0.165);
#7227=CYLINDRICAL_SURFACE('',#8461,0.525);
#7228=CYLINDRICAL_SURFACE('',#8466,0.525);
#7229=CYLINDRICAL_SURFACE('',#8471,0.525);
#7230=CYLINDRICAL_SURFACE('',#8476,0.525);
#7231=CYLINDRICAL_SURFACE('',#8492,0.275);
#7232=CYLINDRICAL_SURFACE('',#8494,0.275);
#7233=CYLINDRICAL_SURFACE('',#8496,0.275);
#7234=CYLINDRICAL_SURFACE('',#8498,0.275);
#7235=CYLINDRICAL_SURFACE('',#8500,2.2);
#7236=CYLINDRICAL_SURFACE('',#8502,1.5);
#7237=CYLINDRICAL_SURFACE('',#8507,2.9);
#7238=CYLINDRICAL_SURFACE('',#8509,1.02);
#7239=CYLINDRICAL_SURFACE('',#8514,0.375);
#7240=CYLINDRICAL_SURFACE('',#8519,0.375);
#7241=CYLINDRICAL_SURFACE('',#8524,0.375);
#7242=CYLINDRICAL_SURFACE('',#8529,0.375);
#7243=CYLINDRICAL_SURFACE('',#8534,0.225);
#7244=CYLINDRICAL_SURFACE('',#8536,0.225);
#7245=CYLINDRICAL_SURFACE('',#8538,0.225);
#7246=CYLINDRICAL_SURFACE('',#8540,0.225);
#7247=CYLINDRICAL_SURFACE('',#8542,1.49);
#7248=CYLINDRICAL_SURFACE('',#8547,0.71);
#7249=CYLINDRICAL_SURFACE('',#8549,2.2);
#7250=CYLINDRICAL_SURFACE('',#8555,0.25);
#7251=CYLINDRICAL_SURFACE('',#8556,0.165);
#7252=CYLINDRICAL_SURFACE('',#8560,0.165);
#7253=CYLINDRICAL_SURFACE('',#8564,0.165);
#7254=CYLINDRICAL_SURFACE('',#8568,0.165);
#7255=CYLINDRICAL_SURFACE('',#8572,0.525);
#7256=CYLINDRICAL_SURFACE('',#8577,0.525);
#7257=CYLINDRICAL_SURFACE('',#8582,0.525);
#7258=CYLINDRICAL_SURFACE('',#8587,0.525);
#7259=CYLINDRICAL_SURFACE('',#8603,0.275);
#7260=CYLINDRICAL_SURFACE('',#8605,0.275);
#7261=CYLINDRICAL_SURFACE('',#8607,0.275);
#7262=CYLINDRICAL_SURFACE('',#8609,0.275);
#7263=CYLINDRICAL_SURFACE('',#8611,2.2);
#7264=CYLINDRICAL_SURFACE('',#8613,1.5);
#7265=CYLINDRICAL_SURFACE('',#8618,2.9);
#7266=CYLINDRICAL_SURFACE('',#8620,1.02);
#7267=CYLINDRICAL_SURFACE('',#8625,0.375);
#7268=CYLINDRICAL_SURFACE('',#8630,0.375);
#7269=CYLINDRICAL_SURFACE('',#8635,0.375);
#7270=CYLINDRICAL_SURFACE('',#8640,0.375);
#7271=CYLINDRICAL_SURFACE('',#8645,0.225);
#7272=CYLINDRICAL_SURFACE('',#8647,0.225);
#7273=CYLINDRICAL_SURFACE('',#8649,0.225);
#7274=CYLINDRICAL_SURFACE('',#8651,0.225);
#7275=CYLINDRICAL_SURFACE('',#8653,1.49);
#7276=CYLINDRICAL_SURFACE('',#8658,0.71);
#7277=CYLINDRICAL_SURFACE('',#8660,2.2);
#7278=CYLINDRICAL_SURFACE('',#8666,0.375);
#7279=CYLINDRICAL_SURFACE('',#8671,0.375);
#7280=CYLINDRICAL_SURFACE('',#8676,0.375);
#7281=CYLINDRICAL_SURFACE('',#8681,0.375);
#7282=CYLINDRICAL_SURFACE('',#8686,0.225);
#7283=CYLINDRICAL_SURFACE('',#8688,0.225);
#7284=CYLINDRICAL_SURFACE('',#8690,0.225);
#7285=CYLINDRICAL_SURFACE('',#8692,0.225000000000001);
#7286=CYLINDRICAL_SURFACE('',#8716,0.976185);
#7287=CYLINDRICAL_SURFACE('',#8718,0.5);
#7288=CYLINDRICAL_SURFACE('',#8724,0.976185);
#7289=CYLINDRICAL_SURFACE('',#8736,1.023815);
#7290=CYLINDRICAL_SURFACE('',#8743,1.5);
#7291=CYLINDRICAL_SURFACE('',#8748,1.023815);
#7292=CYLINDRICAL_SURFACE('',#8770,1.019052);
#7293=CYLINDRICAL_SURFACE('',#8810,0.980948);
#7294=CYLINDRICAL_SURFACE('',#8824,1.013815);
#7295=CYLINDRICAL_SURFACE('',#8828,0.991185);
#7296=CYLINDRICAL_SURFACE('',#8832,1.013815);
#7297=CYLINDRICAL_SURFACE('',#8836,0.991185);
#7298=CYLINDRICAL_SURFACE('',#8844,0.225);
#7299=CYLINDRICAL_SURFACE('',#8847,0.7);
#7300=CYLINDRICAL_SURFACE('',#8858,1.2);
#7301=CYLINDRICAL_SURFACE('',#8860,0.25);
#7302=CYLINDRICAL_SURFACE('',#8862,0.7);
#7303=CYLINDRICAL_SURFACE('',#8868,1.2);
#7304=CYLINDRICAL_SURFACE('',#8872,0.7);
#7305=CYLINDRICAL_SURFACE('',#8873,0.5);
#7306=CYLINDRICAL_SURFACE('',#8877,0.165);
#7307=CYLINDRICAL_SURFACE('',#8881,0.6);
#7308=CYLINDRICAL_SURFACE('',#8887,0.505);
#7309=CYLINDRICAL_SURFACE('',#8890,0.7);
#7310=CYLINDRICAL_SURFACE('',#8898,0.165);
#7311=CYLINDRICAL_SURFACE('',#8901,0.505);
#7312=CYLINDRICAL_SURFACE('',#8904,0.9);
#7313=CYLINDRICAL_SURFACE('',#8910,0.165);
#7314=CYLINDRICAL_SURFACE('',#8920,0.7);
#7315=CYLINDRICAL_SURFACE('',#8921,0.3);
#7316=CYLINDRICAL_SURFACE('',#8923,0.3);
#7317=CYLINDRICAL_SURFACE('',#8928,0.305);
#7318=CYLINDRICAL_SURFACE('',#8931,0.5);
#7319=CYLINDRICAL_SURFACE('',#8937,0.305);
#7320=CYLINDRICAL_SURFACE('',#8940,0.5);
#7321=CYLINDRICAL_SURFACE('',#8946,0.225);
#7322=CYLINDRICAL_SURFACE('',#8949,0.5);
#7323=CYLINDRICAL_SURFACE('',#8959,0.35);
#7324=CYLINDRICAL_SURFACE('',#8967,0.1954);
#7325=CYLINDRICAL_SURFACE('',#8982,0.25);
#7326=CYLINDRICAL_SURFACE('',#8989,1.2);
#7327=CYLINDRICAL_SURFACE('',#8997,1.2);
#7328=CYLINDRICAL_SURFACE('',#9002,0.7);
#7329=CYLINDRICAL_SURFACE('',#9003,0.5);
#7330=CYLINDRICAL_SURFACE('',#9008,0.505);
#7331=CYLINDRICAL_SURFACE('',#9011,0.7);
#7332=CYLINDRICAL_SURFACE('',#9019,0.165);
#7333=CYLINDRICAL_SURFACE('',#9022,0.505);
#7334=CYLINDRICAL_SURFACE('',#9025,0.9);
#7335=CYLINDRICAL_SURFACE('',#9031,0.165);
#7336=CYLINDRICAL_SURFACE('',#9041,0.7);
#7337=CYLINDRICAL_SURFACE('',#9042,0.3);
#7338=CYLINDRICAL_SURFACE('',#9044,0.3);
#7339=CYLINDRICAL_SURFACE('',#9049,0.305);
#7340=CYLINDRICAL_SURFACE('',#9052,0.5);
#7341=CYLINDRICAL_SURFACE('',#9058,0.305);
#7342=CYLINDRICAL_SURFACE('',#9061,0.5);
#7343=CYLINDRICAL_SURFACE('',#9067,0.225);
#7344=CYLINDRICAL_SURFACE('',#9070,0.5);
#7345=CYLINDRICAL_SURFACE('',#9089,0.1954);
#7346=CYLINDRICAL_SURFACE('',#9092,0.305);
#7347=CYLINDRICAL_SURFACE('',#9112,0.5);
#7348=CYLINDRICAL_SURFACE('',#9115,0.5);
#7349=CYLINDRICAL_SURFACE('',#9118,0.800000000000001);
#7350=CYLINDRICAL_SURFACE('',#9125,0.8);
#7351=CYLINDRICAL_SURFACE('',#9129,0.305);
#7352=CYLINDRICAL_SURFACE('',#9132,0.5);
#7353=CYLINDRICAL_SURFACE('',#9138,0.305);
#7354=CYLINDRICAL_SURFACE('',#9141,0.5);
#7355=CYLINDRICAL_SURFACE('',#9151,0.25);
#7356=CYLINDRICAL_SURFACE('',#9154,0.275);
#7357=CYLINDRICAL_SURFACE('',#9157,0.275);
#7358=CYLINDRICAL_SURFACE('',#9160,0.275);
#7359=CYLINDRICAL_SURFACE('',#9163,0.275);
#7360=CYLINDRICAL_SURFACE('',#9173,0.164999999999999);
#7361=CYLINDRICAL_SURFACE('',#9183,0.699999999999999);
#7362=CYLINDRICAL_SURFACE('',#9184,0.300000000000001);
#7363=CYLINDRICAL_SURFACE('',#9186,0.300000000000001);
#7364=CYLINDRICAL_SURFACE('',#9191,0.305);
#7365=CYLINDRICAL_SURFACE('',#9194,0.5);
#7366=CYLINDRICAL_SURFACE('',#9200,0.305);
#7367=CYLINDRICAL_SURFACE('',#9203,0.5);
#7368=CYLINDRICAL_SURFACE('',#9209,0.225);
#7369=CYLINDRICAL_SURFACE('',#9212,0.5);
#7370=CYLINDRICAL_SURFACE('',#9221,0.21);
#7371=CYLINDRICAL_SURFACE('',#9227,0.21);
#7372=CYLINDRICAL_SURFACE('',#9233,0.21);
#7373=CYLINDRICAL_SURFACE('',#9239,0.21);
#7374=CYLINDRICAL_SURFACE('',#9297,0.425);
#7375=CYLINDRICAL_SURFACE('',#9305,0.24505);
#7376=CYLINDRICAL_SURFACE('',#9321,0.35);
#7377=CYLINDRICAL_SURFACE('',#9329,0.1954);
#7378=ADVANCED_FACE('',(#1047),#7210,.F.);
#7379=ADVANCED_FACE('',(#1048),#7211,.F.);
#7380=ADVANCED_FACE('',(#1049),#7212,.F.);
#7381=ADVANCED_FACE('',(#1050),#7213,.F.);
#7382=ADVANCED_FACE('',(#1051),#7214,.F.);
#7383=ADVANCED_FACE('',(#1052),#7215,.F.);
#7384=ADVANCED_FACE('',(#1053),#7216,.F.);
#7385=ADVANCED_FACE('',(#1054),#7217,.F.);
#7386=ADVANCED_FACE('',(#1055),#7218,.F.);
#7387=ADVANCED_FACE('',(#1056),#7219,.F.);
#7388=ADVANCED_FACE('',(#1057),#7220,.F.);
#7389=ADVANCED_FACE('',(#1058),#7221,.F.);
#7390=ADVANCED_FACE('',(#1059),#782,.T.);
#7391=ADVANCED_FACE('',(#1060),#783,.T.);
#7392=ADVANCED_FACE('',(#1061),#784,.T.);
#7393=ADVANCED_FACE('',(#1062),#785,.T.);
#7394=ADVANCED_FACE('',(#1063,#591,#592,#593,#594,#595,#596,#597,#598,#599,
#600,#601,#602),#786,.T.);
#7395=ADVANCED_FACE('',(#1064,#603,#604,#605,#606,#607,#608,#609,#610,#611,
#612,#613,#614),#787,.F.);
#7396=ADVANCED_FACE('',(#1065),#788,.T.);
#7397=ADVANCED_FACE('',(#1066),#789,.T.);
#7398=ADVANCED_FACE('',(#1067),#790,.T.);
#7399=ADVANCED_FACE('',(#1068),#791,.T.);
#7400=ADVANCED_FACE('',(#1069),#792,.T.);
#7401=ADVANCED_FACE('',(#1070),#793,.F.);
#7402=ADVANCED_FACE('',(#1071),#794,.T.);
#7403=ADVANCED_FACE('',(#1072),#795,.T.);
#7404=ADVANCED_FACE('',(#1073),#796,.T.);
#7405=ADVANCED_FACE('',(#1074),#797,.T.);
#7406=ADVANCED_FACE('',(#1075),#798,.T.);
#7407=ADVANCED_FACE('',(#1076),#799,.F.);
#7408=ADVANCED_FACE('',(#1077),#7222,.F.);
#7409=ADVANCED_FACE('',(#1078),#7223,.F.);
#7410=ADVANCED_FACE('',(#1079),#800,.T.);
#7411=ADVANCED_FACE('',(#1080),#7224,.F.);
#7412=ADVANCED_FACE('',(#1081),#801,.T.);
#7413=ADVANCED_FACE('',(#1082),#7225,.F.);
#7414=ADVANCED_FACE('',(#1083),#802,.T.);
#7415=ADVANCED_FACE('',(#1084),#7226,.F.);
#7416=ADVANCED_FACE('',(#1085),#803,.T.);
#7417=ADVANCED_FACE('',(#1086),#7227,.F.);
#7418=ADVANCED_FACE('',(#1087),#804,.F.);
#7419=ADVANCED_FACE('',(#1088),#7228,.F.);
#7420=ADVANCED_FACE('',(#1089),#805,.F.);
#7421=ADVANCED_FACE('',(#1090),#7229,.F.);
#7422=ADVANCED_FACE('',(#1091),#806,.F.);
#7423=ADVANCED_FACE('',(#1092),#7230,.F.);
#7424=ADVANCED_FACE('',(#1093),#807,.F.);
#7425=ADVANCED_FACE('',(#1094,#615,#616,#617,#618,#619),#808,.T.);
#7426=ADVANCED_FACE('',(#1095),#7231,.F.);
#7427=ADVANCED_FACE('',(#1096),#7232,.F.);
#7428=ADVANCED_FACE('',(#1097),#7233,.F.);
#7429=ADVANCED_FACE('',(#1098),#7234,.F.);
#7430=ADVANCED_FACE('',(#1099),#7235,.T.);
#7431=ADVANCED_FACE('',(#1100),#7236,.F.);
#7432=ADVANCED_FACE('',(#1101,#620),#809,.T.);
#7433=ADVANCED_FACE('',(#1102,#621),#7237,.T.);
#7434=ADVANCED_FACE('',(#1103,#622),#7238,.F.);
#7435=ADVANCED_FACE('',(#1104,#623,#624,#625,#626,#627),#810,.T.);
#7436=ADVANCED_FACE('',(#1105,#628,#629,#630,#631,#632),#811,.F.);
#7437=ADVANCED_FACE('',(#1106),#7239,.F.);
#7438=ADVANCED_FACE('',(#1107,#633),#812,.T.);
#7439=ADVANCED_FACE('',(#1108),#7240,.F.);
#7440=ADVANCED_FACE('',(#1109,#634),#813,.T.);
#7441=ADVANCED_FACE('',(#1110),#7241,.F.);
#7442=ADVANCED_FACE('',(#1111,#635),#814,.T.);
#7443=ADVANCED_FACE('',(#1112),#7242,.F.);
#7444=ADVANCED_FACE('',(#1113,#636),#815,.T.);
#7445=ADVANCED_FACE('',(#1114),#7243,.F.);
#7446=ADVANCED_FACE('',(#1115),#7244,.F.);
#7447=ADVANCED_FACE('',(#1116),#7245,.F.);
#7448=ADVANCED_FACE('',(#1117),#7246,.F.);
#7449=ADVANCED_FACE('',(#1118),#7247,.T.);
#7450=ADVANCED_FACE('',(#1119,#637),#816,.F.);
#7451=ADVANCED_FACE('',(#1120),#7248,.F.);
#7452=ADVANCED_FACE('',(#1121),#7249,.T.);
#7453=ADVANCED_FACE('',(#1122,#638,#639,#640,#641,#642),#817,.T.);
#7454=ADVANCED_FACE('',(#1123,#643,#644,#645,#646,#647),#818,.F.);
#7455=ADVANCED_FACE('',(#1124),#7250,.F.);
#7456=ADVANCED_FACE('',(#1125),#7251,.F.);
#7457=ADVANCED_FACE('',(#1126),#819,.T.);
#7458=ADVANCED_FACE('',(#1127),#7252,.F.);
#7459=ADVANCED_FACE('',(#1128),#820,.T.);
#7460=ADVANCED_FACE('',(#1129),#7253,.F.);
#7461=ADVANCED_FACE('',(#1130),#821,.T.);
#7462=ADVANCED_FACE('',(#1131),#7254,.F.);
#7463=ADVANCED_FACE('',(#1132),#822,.T.);
#7464=ADVANCED_FACE('',(#1133),#7255,.F.);
#7465=ADVANCED_FACE('',(#1134),#823,.F.);
#7466=ADVANCED_FACE('',(#1135),#7256,.F.);
#7467=ADVANCED_FACE('',(#1136),#824,.F.);
#7468=ADVANCED_FACE('',(#1137),#7257,.F.);
#7469=ADVANCED_FACE('',(#1138),#825,.F.);
#7470=ADVANCED_FACE('',(#1139),#7258,.F.);
#7471=ADVANCED_FACE('',(#1140),#826,.F.);
#7472=ADVANCED_FACE('',(#1141,#648,#649,#650,#651,#652),#827,.T.);
#7473=ADVANCED_FACE('',(#1142),#7259,.F.);
#7474=ADVANCED_FACE('',(#1143),#7260,.F.);
#7475=ADVANCED_FACE('',(#1144),#7261,.F.);
#7476=ADVANCED_FACE('',(#1145),#7262,.F.);
#7477=ADVANCED_FACE('',(#1146),#7263,.T.);
#7478=ADVANCED_FACE('',(#1147),#7264,.F.);
#7479=ADVANCED_FACE('',(#1148,#653),#828,.T.);
#7480=ADVANCED_FACE('',(#1149,#654),#7265,.T.);
#7481=ADVANCED_FACE('',(#1150,#655),#7266,.F.);
#7482=ADVANCED_FACE('',(#1151,#656,#657,#658,#659,#660),#829,.T.);
#7483=ADVANCED_FACE('',(#1152,#661,#662,#663,#664,#665),#830,.F.);
#7484=ADVANCED_FACE('',(#1153),#7267,.F.);
#7485=ADVANCED_FACE('',(#1154,#666),#831,.T.);
#7486=ADVANCED_FACE('',(#1155),#7268,.F.);
#7487=ADVANCED_FACE('',(#1156,#667),#832,.T.);
#7488=ADVANCED_FACE('',(#1157),#7269,.F.);
#7489=ADVANCED_FACE('',(#1158,#668),#833,.T.);
#7490=ADVANCED_FACE('',(#1159),#7270,.F.);
#7491=ADVANCED_FACE('',(#1160,#669),#834,.T.);
#7492=ADVANCED_FACE('',(#1161),#7271,.F.);
#7493=ADVANCED_FACE('',(#1162),#7272,.F.);
#7494=ADVANCED_FACE('',(#1163),#7273,.F.);
#7495=ADVANCED_FACE('',(#1164),#7274,.F.);
#7496=ADVANCED_FACE('',(#1165),#7275,.T.);
#7497=ADVANCED_FACE('',(#1166,#670),#835,.F.);
#7498=ADVANCED_FACE('',(#1167),#7276,.F.);
#7499=ADVANCED_FACE('',(#1168),#7277,.T.);
#7500=ADVANCED_FACE('',(#1169,#671,#672,#673,#674,#675),#836,.T.);
#7501=ADVANCED_FACE('',(#1170,#676,#677,#678,#679,#680),#837,.F.);
#7502=ADVANCED_FACE('',(#1171),#7278,.F.);
#7503=ADVANCED_FACE('',(#1172,#681),#838,.T.);
#7504=ADVANCED_FACE('',(#1173),#7279,.F.);
#7505=ADVANCED_FACE('',(#1174,#682),#839,.T.);
#7506=ADVANCED_FACE('',(#1175),#7280,.F.);
#7507=ADVANCED_FACE('',(#1176,#683),#840,.T.);
#7508=ADVANCED_FACE('',(#1177),#7281,.F.);
#7509=ADVANCED_FACE('',(#1178,#684),#841,.T.);
#7510=ADVANCED_FACE('',(#1179),#7282,.F.);
#7511=ADVANCED_FACE('',(#1180),#7283,.F.);
#7512=ADVANCED_FACE('',(#1181),#7284,.F.);
#7513=ADVANCED_FACE('',(#1182),#7285,.F.);
#7514=ADVANCED_FACE('',(#1183),#842,.T.);
#7515=ADVANCED_FACE('',(#1184),#843,.T.);
#7516=ADVANCED_FACE('',(#1185),#844,.T.);
#7517=ADVANCED_FACE('',(#1186),#845,.T.);
#7518=ADVANCED_FACE('',(#1187,#685,#686,#687,#688),#846,.T.);
#7519=ADVANCED_FACE('',(#1188),#847,.T.);
#7520=ADVANCED_FACE('',(#1189),#848,.T.);
#7521=ADVANCED_FACE('',(#1190),#849,.T.);
#7522=ADVANCED_FACE('',(#1191),#850,.T.);
#7523=ADVANCED_FACE('',(#1192),#851,.T.);
#7524=ADVANCED_FACE('',(#1193,#689,#690,#691,#692),#852,.T.);
#7525=ADVANCED_FACE('',(#1194),#853,.T.);
#7526=ADVANCED_FACE('',(#1195),#854,.T.);
#7527=ADVANCED_FACE('',(#1196),#855,.F.);
#7528=ADVANCED_FACE('',(#1197),#364,.F.);
#7529=ADVANCED_FACE('',(#1198),#7286,.T.);
#7530=ADVANCED_FACE('',(#1199),#7287,.F.);
#7531=ADVANCED_FACE('',(#1200),#349,.F.);
#7532=ADVANCED_FACE('',(#1201,#693),#856,.T.);
#7533=ADVANCED_FACE('',(#1202),#7288,.T.);
#7534=ADVANCED_FACE('',(#1203,#694),#857,.T.);
#7535=ADVANCED_FACE('',(#1204),#350,.F.);
#7536=ADVANCED_FACE('',(#1205),#365,.F.);
#7537=ADVANCED_FACE('',(#1206),#7289,.F.);
#7538=ADVANCED_FACE('',(#1207,#695),#858,.T.);
#7539=ADVANCED_FACE('',(#1208),#351,.T.);
#7540=ADVANCED_FACE('',(#1209),#7290,.T.);
#7541=ADVANCED_FACE('',(#1210),#352,.T.);
#7542=ADVANCED_FACE('',(#1211,#696),#859,.T.);
#7543=ADVANCED_FACE('',(#1212),#7291,.F.);
#7544=ADVANCED_FACE('',(#1213),#333,.T.);
#7545=ADVANCED_FACE('',(#1214),#334,.T.);
#7546=ADVANCED_FACE('',(#1215),#335,.T.);
#7547=ADVANCED_FACE('',(#1216),#336,.T.);
#7548=ADVANCED_FACE('',(#1217),#337,.T.);
#7549=ADVANCED_FACE('',(#1218),#338,.T.);
#7550=ADVANCED_FACE('',(#1219),#339,.T.);
#7551=ADVANCED_FACE('',(#1220),#340,.T.);
#7552=ADVANCED_FACE('',(#1221),#341,.F.);
#7553=ADVANCED_FACE('',(#1222),#7292,.T.);
#7554=ADVANCED_FACE('',(#1223),#860,.T.);
#7555=ADVANCED_FACE('',(#1224),#342,.F.);
#7556=ADVANCED_FACE('',(#1225),#861,.T.);
#7557=ADVANCED_FACE('',(#1226),#343,.F.);
#7558=ADVANCED_FACE('',(#1227),#862,.T.);
#7559=ADVANCED_FACE('',(#1228),#344,.F.);
#7560=ADVANCED_FACE('',(#1229),#863,.T.);
#7561=ADVANCED_FACE('',(#1230),#345,.F.);
#7562=ADVANCED_FACE('',(#1231),#864,.T.);
#7563=ADVANCED_FACE('',(#1232),#346,.F.);
#7564=ADVANCED_FACE('',(#1233),#865,.T.);
#7565=ADVANCED_FACE('',(#1234),#347,.F.);
#7566=ADVANCED_FACE('',(#1235),#7293,.F.);
#7567=ADVANCED_FACE('',(#1236),#866,.T.);
#7568=ADVANCED_FACE('',(#1237),#348,.F.);
#7569=ADVANCED_FACE('',(#1238,#697),#867,.T.);
#7570=ADVANCED_FACE('',(#1239),#868,.T.);
#7571=ADVANCED_FACE('',(#1240,#698),#869,.T.);
#7572=ADVANCED_FACE('',(#1241),#7294,.T.);
#7573=ADVANCED_FACE('',(#1242,#699),#870,.T.);
#7574=ADVANCED_FACE('',(#1243),#7295,.F.);
#7575=ADVANCED_FACE('',(#1244,#700),#871,.T.);
#7576=ADVANCED_FACE('',(#1245),#7296,.T.);
#7577=ADVANCED_FACE('',(#1246,#701),#872,.T.);
#7578=ADVANCED_FACE('',(#1247),#7297,.F.);
#7579=ADVANCED_FACE('',(#1248),#7298,.F.);
#7580=ADVANCED_FACE('',(#1249),#7299,.T.);
#7581=ADVANCED_FACE('',(#1250),#873,.T.);
#7582=ADVANCED_FACE('',(#1251,#702,#703,#704),#874,.F.);
#7583=ADVANCED_FACE('',(#1252),#875,.T.);
#7584=ADVANCED_FACE('',(#1253),#7300,.T.);
#7585=ADVANCED_FACE('',(#1254),#7301,.F.);
#7586=ADVANCED_FACE('',(#1255),#7302,.T.);
#7587=ADVANCED_FACE('',(#1256),#876,.T.);
#7588=ADVANCED_FACE('',(#1257,#705,#706),#877,.T.);
#7589=ADVANCED_FACE('',(#1258),#878,.T.);
#7590=ADVANCED_FACE('',(#1259),#7303,.T.);
#7591=ADVANCED_FACE('',(#1260,#707),#879,.F.);
#7592=ADVANCED_FACE('',(#1261),#7304,.T.);
#7593=ADVANCED_FACE('',(#1262),#7305,.T.);
#7594=ADVANCED_FACE('',(#1263),#880,.F.);
#7595=ADVANCED_FACE('',(#1264),#7306,.F.);
#7596=ADVANCED_FACE('',(#1265),#881,.T.);
#7597=ADVANCED_FACE('',(#1266),#7307,.T.);
#7598=ADVANCED_FACE('',(#1267,#708),#882,.T.);
#7599=ADVANCED_FACE('',(#1268),#883,.F.);
#7600=ADVANCED_FACE('',(#1269),#7308,.F.);
#7601=ADVANCED_FACE('',(#1270),#7309,.T.);
#7602=ADVANCED_FACE('',(#1271,#709),#884,.T.);
#7603=ADVANCED_FACE('',(#1272,#710),#885,.F.);
#7604=ADVANCED_FACE('',(#1273),#886,.T.);
#7605=ADVANCED_FACE('',(#1274),#7310,.F.);
#7606=ADVANCED_FACE('',(#1275),#887,.T.);
#7607=ADVANCED_FACE('',(#1276,#711),#7311,.F.);
#7608=ADVANCED_FACE('',(#1277,#712),#7312,.T.);
#7609=ADVANCED_FACE('',(#1278,#713),#888,.T.);
#7610=ADVANCED_FACE('',(#1279,#714),#889,.F.);
#7611=ADVANCED_FACE('',(#1280),#7313,.F.);
#7612=ADVANCED_FACE('',(#1281),#890,.T.);
#7613=ADVANCED_FACE('',(#1282,#715),#891,.T.);
#7614=ADVANCED_FACE('',(#1283,#716),#892,.F.);
#7615=ADVANCED_FACE('',(#1284),#7314,.T.);
#7616=ADVANCED_FACE('',(#1285),#7315,.T.);
#7617=ADVANCED_FACE('',(#1286),#7316,.T.);
#7618=ADVANCED_FACE('',(#1287,#717),#893,.T.);
#7619=ADVANCED_FACE('',(#1288),#894,.F.);
#7620=ADVANCED_FACE('',(#1289),#7317,.F.);
#7621=ADVANCED_FACE('',(#1290),#7318,.T.);
#7622=ADVANCED_FACE('',(#1291,#718),#895,.T.);
#7623=ADVANCED_FACE('',(#1292,#719),#896,.F.);
#7624=ADVANCED_FACE('',(#1293),#7319,.F.);
#7625=ADVANCED_FACE('',(#1294),#7320,.T.);
#7626=ADVANCED_FACE('',(#1295,#720),#897,.T.);
#7627=ADVANCED_FACE('',(#1296,#721),#898,.F.);
#7628=ADVANCED_FACE('',(#1297),#7321,.F.);
#7629=ADVANCED_FACE('',(#1298),#7322,.T.);
#7630=ADVANCED_FACE('',(#1299,#722),#899,.T.);
#7631=ADVANCED_FACE('',(#1300,#723),#900,.F.);
#7632=ADVANCED_FACE('',(#1301),#901,.T.);
#7633=ADVANCED_FACE('',(#1302),#353,.T.);
#7634=ADVANCED_FACE('',(#1303),#7323,.T.);
#7635=ADVANCED_FACE('',(#1304),#354,.T.);
#7636=ADVANCED_FACE('',(#1305,#724),#902,.T.);
#7637=ADVANCED_FACE('',(#1306),#355,.T.);
#7638=ADVANCED_FACE('',(#1307),#7324,.T.);
#7639=ADVANCED_FACE('',(#1308),#356,.T.);
#7640=ADVANCED_FACE('',(#1309),#903,.T.);
#7641=ADVANCED_FACE('',(#1310),#904,.F.);
#7642=ADVANCED_FACE('',(#1311),#905,.F.);
#7643=ADVANCED_FACE('',(#1312),#906,.F.);
#7644=ADVANCED_FACE('',(#1313),#907,.F.);
#7645=ADVANCED_FACE('',(#1314),#908,.F.);
#7646=ADVANCED_FACE('',(#1315),#909,.F.);
#7647=ADVANCED_FACE('',(#1316),#910,.F.);
#7648=ADVANCED_FACE('',(#1317),#911,.F.);
#7649=ADVANCED_FACE('',(#1318),#7325,.F.);
#7650=ADVANCED_FACE('',(#1319),#912,.F.);
#7651=ADVANCED_FACE('',(#1320),#913,.F.);
#7652=ADVANCED_FACE('',(#1321),#914,.F.);
#7653=ADVANCED_FACE('',(#1322),#915,.F.);
#7654=ADVANCED_FACE('',(#1323),#7326,.T.);
#7655=ADVANCED_FACE('',(#1324,#725,#726,#727),#916,.F.);
#7656=ADVANCED_FACE('',(#1325),#917,.T.);
#7657=ADVANCED_FACE('',(#1326),#918,.T.);
#7658=ADVANCED_FACE('',(#1327),#7327,.T.);
#7659=ADVANCED_FACE('',(#1328,#728),#919,.F.);
#7660=ADVANCED_FACE('',(#1329),#7328,.T.);
#7661=ADVANCED_FACE('',(#1330),#7329,.T.);
#7662=ADVANCED_FACE('',(#1331,#729,#730),#920,.T.);
#7663=ADVANCED_FACE('',(#1332),#921,.F.);
#7664=ADVANCED_FACE('',(#1333),#7330,.F.);
#7665=ADVANCED_FACE('',(#1334),#7331,.T.);
#7666=ADVANCED_FACE('',(#1335,#731),#922,.T.);
#7667=ADVANCED_FACE('',(#1336,#732),#923,.F.);
#7668=ADVANCED_FACE('',(#1337),#924,.T.);
#7669=ADVANCED_FACE('',(#1338),#7332,.F.);
#7670=ADVANCED_FACE('',(#1339),#925,.T.);
#7671=ADVANCED_FACE('',(#1340,#733),#7333,.F.);
#7672=ADVANCED_FACE('',(#1341,#734),#7334,.T.);
#7673=ADVANCED_FACE('',(#1342,#735),#926,.T.);
#7674=ADVANCED_FACE('',(#1343,#736),#927,.F.);
#7675=ADVANCED_FACE('',(#1344),#7335,.F.);
#7676=ADVANCED_FACE('',(#1345),#928,.T.);
#7677=ADVANCED_FACE('',(#1346,#737),#929,.T.);
#7678=ADVANCED_FACE('',(#1347,#738),#930,.F.);
#7679=ADVANCED_FACE('',(#1348),#7336,.T.);
#7680=ADVANCED_FACE('',(#1349),#7337,.T.);
#7681=ADVANCED_FACE('',(#1350),#7338,.T.);
#7682=ADVANCED_FACE('',(#1351,#739),#931,.T.);
#7683=ADVANCED_FACE('',(#1352),#932,.F.);
#7684=ADVANCED_FACE('',(#1353),#7339,.F.);
#7685=ADVANCED_FACE('',(#1354),#7340,.T.);
#7686=ADVANCED_FACE('',(#1355,#740),#933,.T.);
#7687=ADVANCED_FACE('',(#1356,#741),#934,.F.);
#7688=ADVANCED_FACE('',(#1357),#7341,.F.);
#7689=ADVANCED_FACE('',(#1358),#7342,.T.);
#7690=ADVANCED_FACE('',(#1359,#742),#935,.T.);
#7691=ADVANCED_FACE('',(#1360,#743),#936,.F.);
#7692=ADVANCED_FACE('',(#1361),#7343,.F.);
#7693=ADVANCED_FACE('',(#1362),#7344,.T.);
#7694=ADVANCED_FACE('',(#1363,#744),#937,.T.);
#7695=ADVANCED_FACE('',(#1364,#745),#938,.F.);
#7696=ADVANCED_FACE('',(#1365),#939,.F.);
#7697=ADVANCED_FACE('',(#1366),#940,.F.);
#7698=ADVANCED_FACE('',(#1367),#941,.F.);
#7699=ADVANCED_FACE('',(#1368),#942,.F.);
#7700=ADVANCED_FACE('',(#1369),#943,.F.);
#7701=ADVANCED_FACE('',(#1370),#944,.F.);
#7702=ADVANCED_FACE('',(#1371),#945,.F.);
#7703=ADVANCED_FACE('',(#1372),#946,.F.);
#7704=ADVANCED_FACE('',(#1373,#746),#947,.T.);
#7705=ADVANCED_FACE('',(#1374),#357,.T.);
#7706=ADVANCED_FACE('',(#1375),#7345,.T.);
#7707=ADVANCED_FACE('',(#1376),#7346,.F.);
#7708=ADVANCED_FACE('',(#1377),#948,.F.);
#7709=ADVANCED_FACE('',(#1378),#949,.F.);
#7710=ADVANCED_FACE('',(#1379),#950,.T.);
#7711=ADVANCED_FACE('',(#1380),#951,.T.);
#7712=ADVANCED_FACE('',(#1381,#747),#952,.T.);
#7713=ADVANCED_FACE('',(#1382),#953,.T.);
#7714=ADVANCED_FACE('',(#1383),#954,.T.);
#7715=ADVANCED_FACE('',(#1384),#955,.T.);
#7716=ADVANCED_FACE('',(#1385),#956,.T.);
#7717=ADVANCED_FACE('',(#1386,#748),#957,.F.);
#7718=ADVANCED_FACE('',(#1387),#958,.T.);
#7719=ADVANCED_FACE('',(#1388),#959,.T.);
#7720=ADVANCED_FACE('',(#1389),#960,.T.);
#7721=ADVANCED_FACE('',(#1390),#961,.T.);
#7722=ADVANCED_FACE('',(#1391),#7347,.F.);
#7723=ADVANCED_FACE('',(#1392),#7348,.F.);
#7724=ADVANCED_FACE('',(#1393),#7349,.T.);
#7725=ADVANCED_FACE('',(#1394),#962,.T.);
#7726=ADVANCED_FACE('',(#1395,#749,#750),#963,.F.);
#7727=ADVANCED_FACE('',(#1396),#964,.T.);
#7728=ADVANCED_FACE('',(#1397),#7350,.T.);
#7729=ADVANCED_FACE('',(#1398,#751,#752),#965,.T.);
#7730=ADVANCED_FACE('',(#1399),#7351,.F.);
#7731=ADVANCED_FACE('',(#1400),#7352,.T.);
#7732=ADVANCED_FACE('',(#1401,#753),#966,.T.);
#7733=ADVANCED_FACE('',(#1402,#754),#967,.F.);
#7734=ADVANCED_FACE('',(#1403),#7353,.F.);
#7735=ADVANCED_FACE('',(#1404),#7354,.T.);
#7736=ADVANCED_FACE('',(#1405,#755),#968,.T.);
#7737=ADVANCED_FACE('',(#1406,#756),#969,.F.);
#7738=ADVANCED_FACE('',(#1407),#7355,.F.);
#7739=ADVANCED_FACE('',(#1408),#7356,.F.);
#7740=ADVANCED_FACE('',(#1409),#7357,.F.);
#7741=ADVANCED_FACE('',(#1410),#7358,.F.);
#7742=ADVANCED_FACE('',(#1411),#7359,.F.);
#7743=ADVANCED_FACE('',(#1412),#970,.T.);
#7744=ADVANCED_FACE('',(#1413),#971,.T.);
#7745=ADVANCED_FACE('',(#1414),#972,.T.);
#7746=ADVANCED_FACE('',(#1415),#973,.T.);
#7747=ADVANCED_FACE('',(#1416,#757,#758,#759,#760,#761),#974,.T.);
#7748=ADVANCED_FACE('',(#1417,#762,#763,#764,#765,#766),#975,.F.);
#7749=ADVANCED_FACE('',(#1418),#7360,.F.);
#7750=ADVANCED_FACE('',(#1419),#976,.T.);
#7751=ADVANCED_FACE('',(#1420,#767),#977,.T.);
#7752=ADVANCED_FACE('',(#1421,#768),#978,.F.);
#7753=ADVANCED_FACE('',(#1422),#7361,.T.);
#7754=ADVANCED_FACE('',(#1423),#7362,.T.);
#7755=ADVANCED_FACE('',(#1424),#7363,.T.);
#7756=ADVANCED_FACE('',(#1425,#769),#979,.T.);
#7757=ADVANCED_FACE('',(#1426),#980,.F.);
#7758=ADVANCED_FACE('',(#1427),#7364,.F.);
#7759=ADVANCED_FACE('',(#1428),#7365,.T.);
#7760=ADVANCED_FACE('',(#1429,#770),#981,.T.);
#7761=ADVANCED_FACE('',(#1430,#771),#982,.F.);
#7762=ADVANCED_FACE('',(#1431),#7366,.F.);
#7763=ADVANCED_FACE('',(#1432),#7367,.T.);
#7764=ADVANCED_FACE('',(#1433,#772),#983,.T.);
#7765=ADVANCED_FACE('',(#1434,#773),#984,.F.);
#7766=ADVANCED_FACE('',(#1435),#7368,.F.);
#7767=ADVANCED_FACE('',(#1436),#7369,.T.);
#7768=ADVANCED_FACE('',(#1437,#774),#985,.T.);
#7769=ADVANCED_FACE('',(#1438,#775),#986,.F.);
#7770=ADVANCED_FACE('',(#1439),#987,.T.);
#7771=ADVANCED_FACE('',(#1440),#7370,.F.);
#7772=ADVANCED_FACE('',(#1441),#988,.T.);
#7773=ADVANCED_FACE('',(#1442),#7371,.F.);
#7774=ADVANCED_FACE('',(#1443),#989,.T.);
#7775=ADVANCED_FACE('',(#1444),#7372,.F.);
#7776=ADVANCED_FACE('',(#1445),#990,.T.);
#7777=ADVANCED_FACE('',(#1446),#7373,.F.);
#7778=ADVANCED_FACE('',(#1447),#991,.T.);
#7779=ADVANCED_FACE('',(#1448),#992,.T.);
#7780=ADVANCED_FACE('',(#1449),#993,.T.);
#7781=ADVANCED_FACE('',(#1450),#994,.T.);
#7782=ADVANCED_FACE('',(#1451),#995,.T.);
#7783=ADVANCED_FACE('',(#1452,#776,#777,#778,#779),#996,.T.);
#7784=ADVANCED_FACE('',(#1453),#997,.T.);
#7785=ADVANCED_FACE('',(#1454),#998,.T.);
#7786=ADVANCED_FACE('',(#1455),#999,.T.);
#7787=ADVANCED_FACE('',(#1456),#1000,.T.);
#7788=ADVANCED_FACE('',(#1457),#1001,.T.);
#7789=ADVANCED_FACE('',(#1458),#1002,.T.);
#7790=ADVANCED_FACE('',(#1459),#1003,.T.);
#7791=ADVANCED_FACE('',(#1460),#1004,.T.);
#7792=ADVANCED_FACE('',(#1461),#1005,.T.);
#7793=ADVANCED_FACE('',(#1462),#1006,.T.);
#7794=ADVANCED_FACE('',(#1463),#1007,.T.);
#7795=ADVANCED_FACE('',(#1464),#1008,.T.);
#7796=ADVANCED_FACE('',(#1465),#1009,.T.);
#7797=ADVANCED_FACE('',(#1466),#1010,.T.);
#7798=ADVANCED_FACE('',(#1467),#1011,.T.);
#7799=ADVANCED_FACE('',(#1468),#1012,.T.);
#7800=ADVANCED_FACE('',(#1469),#1013,.T.);
#7801=ADVANCED_FACE('',(#1470),#1014,.F.);
#7802=ADVANCED_FACE('',(#1471),#1015,.T.);
#7803=ADVANCED_FACE('',(#1472),#1016,.T.);
#7804=ADVANCED_FACE('',(#1473),#1017,.T.);
#7805=ADVANCED_FACE('',(#1474),#1018,.T.);
#7806=ADVANCED_FACE('',(#1475),#1019,.T.);
#7807=ADVANCED_FACE('',(#1476),#1020,.T.);
#7808=ADVANCED_FACE('',(#1477),#1021,.T.);
#7809=ADVANCED_FACE('',(#1478),#1022,.T.);
#7810=ADVANCED_FACE('',(#1479),#1023,.T.);
#7811=ADVANCED_FACE('',(#1480),#1024,.T.);
#7812=ADVANCED_FACE('',(#1481),#1025,.F.);
#7813=ADVANCED_FACE('',(#1482),#1026,.F.);
#7814=ADVANCED_FACE('',(#1483),#1027,.F.);
#7815=ADVANCED_FACE('',(#1484),#1028,.F.);
#7816=ADVANCED_FACE('',(#1485),#1029,.F.);
#7817=ADVANCED_FACE('',(#1486),#1030,.F.);
#7818=ADVANCED_FACE('',(#1487),#1031,.F.);
#7819=ADVANCED_FACE('',(#1488),#1032,.F.);
#7820=ADVANCED_FACE('',(#1489),#1033,.F.);
#7821=ADVANCED_FACE('',(#1490),#1034,.T.);
#7822=ADVANCED_FACE('',(#1491),#358,.T.);
#7823=ADVANCED_FACE('',(#1492),#7374,.T.);
#7824=ADVANCED_FACE('',(#1493),#359,.T.);
#7825=ADVANCED_FACE('',(#1494,#780),#1035,.T.);
#7826=ADVANCED_FACE('',(#1495),#360,.T.);
#7827=ADVANCED_FACE('',(#1496),#7375,.T.);
#7828=ADVANCED_FACE('',(#1497),#1036,.F.);
#7829=ADVANCED_FACE('',(#1498),#1037,.F.);
#7830=ADVANCED_FACE('',(#1499),#1038,.F.);
#7831=ADVANCED_FACE('',(#1500),#1039,.F.);
#7832=ADVANCED_FACE('',(#1501),#1040,.F.);
#7833=ADVANCED_FACE('',(#1502),#1041,.F.);
#7834=ADVANCED_FACE('',(#1503),#1042,.F.);
#7835=ADVANCED_FACE('',(#1504),#1043,.F.);
#7836=ADVANCED_FACE('',(#1505),#1044,.F.);
#7837=ADVANCED_FACE('',(#1506),#1045,.T.);
#7838=ADVANCED_FACE('',(#1507),#361,.T.);
#7839=ADVANCED_FACE('',(#1508),#7376,.T.);
#7840=ADVANCED_FACE('',(#1509),#362,.T.);
#7841=ADVANCED_FACE('',(#1510,#781),#1046,.T.);
#7842=ADVANCED_FACE('',(#1511),#363,.T.);
#7843=ADVANCED_FACE('',(#1512),#7377,.T.);
#7844=CLOSED_SHELL('',(#7378,#7379,#7380,#7381,#7382,#7383,#7384,#7385,
#7386,#7387,#7388,#7389,#7390,#7391,#7392,#7393,#7394,#7395));
#7845=CLOSED_SHELL('',(#7396,#7397,#7398,#7399,#7400,#7401));
#7846=CLOSED_SHELL('',(#7402,#7403,#7404,#7405,#7406,#7407));
#7847=CLOSED_SHELL('',(#7408,#7409,#7410,#7411,#7412,#7413,#7414,#7415,
#7416,#7417,#7418,#7419,#7420,#7421,#7422,#7423,#7424,#7425,#7426,#7427,
#7428,#7429,#7430,#7431,#7432,#7433,#7434,#7435,#7436));
#7848=CLOSED_SHELL('',(#7437,#7438,#7439,#7440,#7441,#7442,#7443,#7444,
#7445,#7446,#7447,#7448,#7449,#7450,#7451,#7452,#7453,#7454));
#7849=CLOSED_SHELL('',(#7455,#7456,#7457,#7458,#7459,#7460,#7461,#7462,
#7463,#7464,#7465,#7466,#7467,#7468,#7469,#7470,#7471,#7472,#7473,#7474,
#7475,#7476,#7477,#7478,#7479,#7480,#7481,#7482,#7483));
#7850=CLOSED_SHELL('',(#7484,#7485,#7486,#7487,#7488,#7489,#7490,#7491,
#7492,#7493,#7494,#7495,#7496,#7497,#7498,#7499,#7500,#7501));
#7851=CLOSED_SHELL('',(#7502,#7503,#7504,#7505,#7506,#7507,#7508,#7509,
#7510,#7511,#7512,#7513,#7514,#7515,#7516,#7517,#7518,#7519,#7520,#7521,
#7522,#7523,#7524,#7525,#7526,#7527));
#7852=CLOSED_SHELL('',(#7528,#7529,#7530,#7531,#7532,#7533,#7534,#7535));
#7853=CLOSED_SHELL('',(#7536,#7537,#7538,#7539,#7540,#7541,#7542,#7543));
#7854=CLOSED_SHELL('',(#7544));
#7855=CLOSED_SHELL('',(#7545));
#7856=CLOSED_SHELL('',(#7546));
#7857=CLOSED_SHELL('',(#7547));
#7858=CLOSED_SHELL('',(#7548));
#7859=CLOSED_SHELL('',(#7549));
#7860=CLOSED_SHELL('',(#7550));
#7861=CLOSED_SHELL('',(#7551));
#7862=CLOSED_SHELL('',(#7552,#7553,#7554,#7555,#7556,#7557,#7558,#7559,
#7560,#7561,#7562,#7563,#7564,#7565,#7566,#7567,#7568,#7569,#7570));
#7863=CLOSED_SHELL('',(#7571,#7572,#7573,#7574));
#7864=CLOSED_SHELL('',(#7575,#7576,#7577,#7578));
#7865=CLOSED_SHELL('',(#7579,#7580,#7581,#7582,#7583,#7584,#7585,#7586,
#7587,#7588,#7589,#7590,#7591,#7592,#7593,#7594));
#7866=CLOSED_SHELL('',(#7595,#7596,#7597,#7598,#7599));
#7867=CLOSED_SHELL('',(#7600,#7601,#7602,#7603));
#7868=CLOSED_SHELL('',(#7604,#7605,#7606,#7607,#7608,#7609,#7610));
#7869=CLOSED_SHELL('',(#7611,#7612,#7613,#7614,#7615,#7616,#7617,#7618,
#7619));
#7870=CLOSED_SHELL('',(#7620,#7621,#7622,#7623));
#7871=CLOSED_SHELL('',(#7624,#7625,#7626,#7627));
#7872=CLOSED_SHELL('',(#7628,#7629,#7630,#7631));
#7873=CLOSED_SHELL('',(#7632,#7633,#7634,#7635,#7636,#7637,#7638,#7639,
#7640));
#7874=CLOSED_SHELL('',(#7641,#7642,#7643,#7644,#7645,#7646,#7647,#7648));
#7875=CLOSED_SHELL('',(#7649,#7650,#7651,#7652,#7653,#7654,#7655,#7656,
#7657,#7658,#7659,#7660,#7661,#7662,#7663));
#7876=CLOSED_SHELL('',(#7664,#7665,#7666,#7667));
#7877=CLOSED_SHELL('',(#7668,#7669,#7670,#7671,#7672,#7673,#7674));
#7878=CLOSED_SHELL('',(#7675,#7676,#7677,#7678,#7679,#7680,#7681,#7682,
#7683));
#7879=CLOSED_SHELL('',(#7684,#7685,#7686,#7687));
#7880=CLOSED_SHELL('',(#7688,#7689,#7690,#7691));
#7881=CLOSED_SHELL('',(#7692,#7693,#7694,#7695));
#7882=CLOSED_SHELL('',(#7696,#7697,#7698,#7699,#7700,#7701,#7702,#7703,
#7704,#7705,#7706));
#7883=CLOSED_SHELL('',(#7707,#7708,#7709,#7710,#7711,#7712,#7713,#7714,
#7715,#7716,#7717,#7718,#7719,#7720,#7721));
#7884=CLOSED_SHELL('',(#7722,#7723,#7724,#7725,#7726,#7727,#7728,#7729));
#7885=CLOSED_SHELL('',(#7730,#7731,#7732,#7733));
#7886=CLOSED_SHELL('',(#7734,#7735,#7736,#7737));
#7887=CLOSED_SHELL('',(#7738,#7739,#7740,#7741,#7742,#7743,#7744,#7745,
#7746,#7747,#7748));
#7888=CLOSED_SHELL('',(#7749,#7750,#7751,#7752,#7753,#7754,#7755,#7756,
#7757));
#7889=CLOSED_SHELL('',(#7758,#7759,#7760,#7761));
#7890=CLOSED_SHELL('',(#7762,#7763,#7764,#7765));
#7891=CLOSED_SHELL('',(#7766,#7767,#7768,#7769));
#7892=CLOSED_SHELL('',(#7770,#7771,#7772,#7773,#7774,#7775,#7776,#7777,
#7778,#7779,#7780,#7781,#7782,#7783,#7784,#7785,#7786,#7787,#7788,#7789,
#7790,#7791));
#7893=CLOSED_SHELL('',(#7792,#7793,#7794,#7795,#7796,#7797,#7798,#7799,
#7800,#7801));
#7894=CLOSED_SHELL('',(#7802,#7803,#7804,#7805,#7806,#7807,#7808,#7809,
#7810,#7811));
#7895=CLOSED_SHELL('',(#7812,#7813,#7814,#7815,#7816,#7817,#7818,#7819));
#7896=CLOSED_SHELL('',(#7820,#7821,#7822,#7823,#7824,#7825,#7826,#7827));
#7897=CLOSED_SHELL('',(#7828,#7829,#7830,#7831,#7832,#7833,#7834,#7835));
#7898=CLOSED_SHELL('',(#7836,#7837,#7838,#7839,#7840,#7841,#7842,#7843));
#7899=DERIVED_UNIT_ELEMENT(#7987,1.);
#7900=DERIVED_UNIT_ELEMENT(#14880,-3.);
#7901=DERIVED_UNIT_ELEMENT(#7987,1.);
#7902=DERIVED_UNIT_ELEMENT(#14880,-3.);
#7903=DERIVED_UNIT_ELEMENT(#7987,1.);
#7904=DERIVED_UNIT_ELEMENT(#14880,-3.);
#7905=DERIVED_UNIT_ELEMENT(#7987,1.);
#7906=DERIVED_UNIT_ELEMENT(#14880,-3.);
#7907=DERIVED_UNIT_ELEMENT(#7987,1.);
#7908=DERIVED_UNIT_ELEMENT(#14880,-3.);
#7909=DERIVED_UNIT_ELEMENT(#7987,1.);
#7910=DERIVED_UNIT_ELEMENT(#14880,-3.);
#7911=DERIVED_UNIT_ELEMENT(#7987,1.);
#7912=DERIVED_UNIT_ELEMENT(#14880,-3.);
#7913=DERIVED_UNIT_ELEMENT(#7987,1.);
#7914=DERIVED_UNIT_ELEMENT(#14880,-3.);
#7915=DERIVED_UNIT_ELEMENT(#7987,1.);
#7916=DERIVED_UNIT_ELEMENT(#14880,-3.);
#7917=DERIVED_UNIT_ELEMENT(#7987,1.);
#7918=DERIVED_UNIT_ELEMENT(#14880,-3.);
#7919=DERIVED_UNIT_ELEMENT(#7987,1.);
#7920=DERIVED_UNIT_ELEMENT(#14880,-3.);
#7921=DERIVED_UNIT_ELEMENT(#7987,1.);
#7922=DERIVED_UNIT_ELEMENT(#14880,-3.);
#7923=DERIVED_UNIT_ELEMENT(#7987,1.);
#7924=DERIVED_UNIT_ELEMENT(#14880,-3.);
#7925=DERIVED_UNIT_ELEMENT(#7987,1.);
#7926=DERIVED_UNIT_ELEMENT(#14880,-3.);
#7927=DERIVED_UNIT_ELEMENT(#7987,1.);
#7928=DERIVED_UNIT_ELEMENT(#14880,-3.);
#7929=DERIVED_UNIT_ELEMENT(#7987,1.);
#7930=DERIVED_UNIT_ELEMENT(#14880,-3.);
#7931=DERIVED_UNIT_ELEMENT(#7987,1.);
#7932=DERIVED_UNIT_ELEMENT(#14880,-3.);
#7933=DERIVED_UNIT_ELEMENT(#7987,1.);
#7934=DERIVED_UNIT_ELEMENT(#14880,-3.);
#7935=DERIVED_UNIT_ELEMENT(#7987,1.);
#7936=DERIVED_UNIT_ELEMENT(#14880,-3.);
#7937=DERIVED_UNIT_ELEMENT(#7987,1.);
#7938=DERIVED_UNIT_ELEMENT(#14880,-3.);
#7939=DERIVED_UNIT_ELEMENT(#7987,1.);
#7940=DERIVED_UNIT_ELEMENT(#14880,-3.);
#7941=DERIVED_UNIT_ELEMENT(#7987,1.);
#7942=DERIVED_UNIT_ELEMENT(#14880,-3.);
#7943=DERIVED_UNIT_ELEMENT(#7987,1.);
#7944=DERIVED_UNIT_ELEMENT(#14880,-3.);
#7945=DERIVED_UNIT_ELEMENT(#7987,1.);
#7946=DERIVED_UNIT_ELEMENT(#14880,-3.);
#7947=DERIVED_UNIT_ELEMENT(#7987,1.);
#7948=DERIVED_UNIT_ELEMENT(#14880,-3.);
#7949=DERIVED_UNIT_ELEMENT(#7987,1.);
#7950=DERIVED_UNIT_ELEMENT(#14880,-3.);
#7951=DERIVED_UNIT_ELEMENT(#7987,1.);
#7952=DERIVED_UNIT_ELEMENT(#14880,-3.);
#7953=DERIVED_UNIT_ELEMENT(#7987,1.);
#7954=DERIVED_UNIT_ELEMENT(#14880,-3.);
#7955=DERIVED_UNIT_ELEMENT(#7987,1.);
#7956=DERIVED_UNIT_ELEMENT(#14880,-3.);
#7957=DERIVED_UNIT_ELEMENT(#7987,1.);
#7958=DERIVED_UNIT_ELEMENT(#14880,-3.);
#7959=DERIVED_UNIT_ELEMENT(#7987,1.);
#7960=DERIVED_UNIT_ELEMENT(#14880,-3.);
#7961=DERIVED_UNIT_ELEMENT(#7987,1.);
#7962=DERIVED_UNIT_ELEMENT(#14880,-3.);
#7963=DERIVED_UNIT_ELEMENT(#7987,1.);
#7964=DERIVED_UNIT_ELEMENT(#14880,-3.);
#7965=DERIVED_UNIT_ELEMENT(#7987,1.);
#7966=DERIVED_UNIT_ELEMENT(#14880,-3.);
#7967=DERIVED_UNIT_ELEMENT(#7987,1.);
#7968=DERIVED_UNIT_ELEMENT(#14880,-3.);
#7969=DERIVED_UNIT_ELEMENT(#7987,1.);
#7970=DERIVED_UNIT_ELEMENT(#14880,-3.);
#7971=DERIVED_UNIT_ELEMENT(#7987,1.);
#7972=DERIVED_UNIT_ELEMENT(#14880,-3.);
#7973=DERIVED_UNIT_ELEMENT(#7987,1.);
#7974=DERIVED_UNIT_ELEMENT(#14880,-3.);
#7975=DERIVED_UNIT_ELEMENT(#7987,1.);
#7976=DERIVED_UNIT_ELEMENT(#14880,-3.);
#7977=DERIVED_UNIT_ELEMENT(#7987,1.);
#7978=DERIVED_UNIT_ELEMENT(#14880,-3.);
#7979=DERIVED_UNIT_ELEMENT(#7987,1.);
#7980=DERIVED_UNIT_ELEMENT(#14880,-3.);
#7981=DERIVED_UNIT_ELEMENT(#7987,1.);
#7982=DERIVED_UNIT_ELEMENT(#14880,-3.);
#7983=DERIVED_UNIT_ELEMENT(#7987,1.);
#7984=DERIVED_UNIT_ELEMENT(#14880,-3.);
#7985=DERIVED_UNIT_ELEMENT(#7987,1.);
#7986=DERIVED_UNIT_ELEMENT(#14880,-3.);
#7987=(
MASS_UNIT()
NAMED_UNIT(*)
SI_UNIT(.KILO.,.GRAM.)
);
#7988=DERIVED_UNIT((#7899,#7900));
#7989=DERIVED_UNIT((#7901,#7902));
#7990=DERIVED_UNIT((#7903,#7904));
#7991=DERIVED_UNIT((#7905,#7906));
#7992=DERIVED_UNIT((#7907,#7908));
#7993=DERIVED_UNIT((#7909,#7910));
#7994=DERIVED_UNIT((#7911,#7912));
#7995=DERIVED_UNIT((#7913,#7914));
#7996=DERIVED_UNIT((#7915,#7916));
#7997=DERIVED_UNIT((#7917,#7918));
#7998=DERIVED_UNIT((#7919,#7920));
#7999=DERIVED_UNIT((#7921,#7922));
#8000=DERIVED_UNIT((#7923,#7924));
#8001=DERIVED_UNIT((#7925,#7926));
#8002=DERIVED_UNIT((#7927,#7928));
#8003=DERIVED_UNIT((#7929,#7930));
#8004=DERIVED_UNIT((#7931,#7932));
#8005=DERIVED_UNIT((#7933,#7934));
#8006=DERIVED_UNIT((#7935,#7936));
#8007=DERIVED_UNIT((#7937,#7938));
#8008=DERIVED_UNIT((#7939,#7940));
#8009=DERIVED_UNIT((#7941,#7942));
#8010=DERIVED_UNIT((#7943,#7944));
#8011=DERIVED_UNIT((#7945,#7946));
#8012=DERIVED_UNIT((#7947,#7948));
#8013=DERIVED_UNIT((#7949,#7950));
#8014=DERIVED_UNIT((#7951,#7952));
#8015=DERIVED_UNIT((#7953,#7954));
#8016=DERIVED_UNIT((#7955,#7956));
#8017=DERIVED_UNIT((#7957,#7958));
#8018=DERIVED_UNIT((#7959,#7960));
#8019=DERIVED_UNIT((#7961,#7962));
#8020=DERIVED_UNIT((#7963,#7964));
#8021=DERIVED_UNIT((#7965,#7966));
#8022=DERIVED_UNIT((#7967,#7968));
#8023=DERIVED_UNIT((#7969,#7970));
#8024=DERIVED_UNIT((#7971,#7972));
#8025=DERIVED_UNIT((#7973,#7974));
#8026=DERIVED_UNIT((#7975,#7976));
#8027=DERIVED_UNIT((#7977,#7978));
#8028=DERIVED_UNIT((#7979,#7980));
#8029=DERIVED_UNIT((#7981,#7982));
#8030=DERIVED_UNIT((#7983,#7984));
#8031=DERIVED_UNIT((#7985,#7986));
#8032=MEASURE_REPRESENTATION_ITEM('density measure',
POSITIVE_RATIO_MEASURE(7850.),#7988);
#8033=MEASURE_REPRESENTATION_ITEM('density measure',
POSITIVE_RATIO_MEASURE(7850.),#7989);
#8034=MEASURE_REPRESENTATION_ITEM('density measure',
POSITIVE_RATIO_MEASURE(7850.),#7990);
#8035=MEASURE_REPRESENTATION_ITEM('density measure',
POSITIVE_RATIO_MEASURE(7850.),#7991);
#8036=MEASURE_REPRESENTATION_ITEM('density measure',
POSITIVE_RATIO_MEASURE(7850.),#7992);
#8037=MEASURE_REPRESENTATION_ITEM('density measure',
POSITIVE_RATIO_MEASURE(7850.),#7993);
#8038=MEASURE_REPRESENTATION_ITEM('density measure',
POSITIVE_RATIO_MEASURE(7850.),#7994);
#8039=MEASURE_REPRESENTATION_ITEM('density measure',
POSITIVE_RATIO_MEASURE(7850.),#7995);
#8040=MEASURE_REPRESENTATION_ITEM('density measure',
POSITIVE_RATIO_MEASURE(7850.),#7996);
#8041=MEASURE_REPRESENTATION_ITEM('density measure',
POSITIVE_RATIO_MEASURE(7850.),#7997);
#8042=MEASURE_REPRESENTATION_ITEM('density measure',
POSITIVE_RATIO_MEASURE(7850.),#7998);
#8043=MEASURE_REPRESENTATION_ITEM('density measure',
POSITIVE_RATIO_MEASURE(7850.),#7999);
#8044=MEASURE_REPRESENTATION_ITEM('density measure',
POSITIVE_RATIO_MEASURE(7850.),#8000);
#8045=MEASURE_REPRESENTATION_ITEM('density measure',
POSITIVE_RATIO_MEASURE(7850.),#8001);
#8046=MEASURE_REPRESENTATION_ITEM('density measure',
POSITIVE_RATIO_MEASURE(7850.),#8002);
#8047=MEASURE_REPRESENTATION_ITEM('density measure',
POSITIVE_RATIO_MEASURE(7850.),#8003);
#8048=MEASURE_REPRESENTATION_ITEM('density measure',
POSITIVE_RATIO_MEASURE(7850.),#8004);
#8049=MEASURE_REPRESENTATION_ITEM('density measure',
POSITIVE_RATIO_MEASURE(7850.),#8005);
#8050=MEASURE_REPRESENTATION_ITEM('density measure',
POSITIVE_RATIO_MEASURE(7850.),#8006);
#8051=MEASURE_REPRESENTATION_ITEM('density measure',
POSITIVE_RATIO_MEASURE(7850.),#8007);
#8052=MEASURE_REPRESENTATION_ITEM('density measure',
POSITIVE_RATIO_MEASURE(7850.),#8008);
#8053=MEASURE_REPRESENTATION_ITEM('density measure',
POSITIVE_RATIO_MEASURE(7850.),#8009);
#8054=MEASURE_REPRESENTATION_ITEM('density measure',
POSITIVE_RATIO_MEASURE(7850.),#8010);
#8055=MEASURE_REPRESENTATION_ITEM('density measure',
POSITIVE_RATIO_MEASURE(7850.),#8011);
#8056=MEASURE_REPRESENTATION_ITEM('density measure',
POSITIVE_RATIO_MEASURE(7850.),#8012);
#8057=MEASURE_REPRESENTATION_ITEM('density measure',
POSITIVE_RATIO_MEASURE(7850.),#8013);
#8058=MEASURE_REPRESENTATION_ITEM('density measure',
POSITIVE_RATIO_MEASURE(7850.),#8014);
#8059=MEASURE_REPRESENTATION_ITEM('density measure',
POSITIVE_RATIO_MEASURE(7850.),#8015);
#8060=MEASURE_REPRESENTATION_ITEM('density measure',
POSITIVE_RATIO_MEASURE(7850.),#8016);
#8061=MEASURE_REPRESENTATION_ITEM('density measure',
POSITIVE_RATIO_MEASURE(7850.),#8017);
#8062=MEASURE_REPRESENTATION_ITEM('density measure',
POSITIVE_RATIO_MEASURE(7850.),#8018);
#8063=MEASURE_REPRESENTATION_ITEM('density measure',
POSITIVE_RATIO_MEASURE(7850.),#8019);
#8064=MEASURE_REPRESENTATION_ITEM('density measure',
POSITIVE_RATIO_MEASURE(7850.),#8020);
#8065=MEASURE_REPRESENTATION_ITEM('density measure',
POSITIVE_RATIO_MEASURE(7850.),#8021);
#8066=MEASURE_REPRESENTATION_ITEM('density measure',
POSITIVE_RATIO_MEASURE(7850.),#8022);
#8067=MEASURE_REPRESENTATION_ITEM('density measure',
POSITIVE_RATIO_MEASURE(7850.),#8023);
#8068=MEASURE_REPRESENTATION_ITEM('density measure',
POSITIVE_RATIO_MEASURE(7850.),#8024);
#8069=MEASURE_REPRESENTATION_ITEM('density measure',
POSITIVE_RATIO_MEASURE(7850.),#8025);
#8070=MEASURE_REPRESENTATION_ITEM('density measure',
POSITIVE_RATIO_MEASURE(7850.),#8026);
#8071=MEASURE_REPRESENTATION_ITEM('density measure',
POSITIVE_RATIO_MEASURE(7850.),#8027);
#8072=MEASURE_REPRESENTATION_ITEM('density measure',
POSITIVE_RATIO_MEASURE(7850.),#8028);
#8073=MEASURE_REPRESENTATION_ITEM('density measure',
POSITIVE_RATIO_MEASURE(7850.),#8029);
#8074=MEASURE_REPRESENTATION_ITEM('density measure',
POSITIVE_RATIO_MEASURE(7850.),#8030);
#8075=MEASURE_REPRESENTATION_ITEM('density measure',
POSITIVE_RATIO_MEASURE(7850.),#8031);
#8076=PROPERTY_DEFINITION_REPRESENTATION(#8296,#8164);
#8077=PROPERTY_DEFINITION_REPRESENTATION(#8297,#8165);
#8078=PROPERTY_DEFINITION_REPRESENTATION(#8298,#8166);
#8079=PROPERTY_DEFINITION_REPRESENTATION(#8299,#8167);
#8080=PROPERTY_DEFINITION_REPRESENTATION(#8300,#8168);
#8081=PROPERTY_DEFINITION_REPRESENTATION(#8301,#8169);
#8082=PROPERTY_DEFINITION_REPRESENTATION(#8302,#8170);
#8083=PROPERTY_DEFINITION_REPRESENTATION(#8303,#8171);
#8084=PROPERTY_DEFINITION_REPRESENTATION(#8304,#8172);
#8085=PROPERTY_DEFINITION_REPRESENTATION(#8305,#8173);
#8086=PROPERTY_DEFINITION_REPRESENTATION(#8306,#8174);
#8087=PROPERTY_DEFINITION_REPRESENTATION(#8307,#8175);
#8088=PROPERTY_DEFINITION_REPRESENTATION(#8308,#8176);
#8089=PROPERTY_DEFINITION_REPRESENTATION(#8309,#8177);
#8090=PROPERTY_DEFINITION_REPRESENTATION(#8310,#8178);
#8091=PROPERTY_DEFINITION_REPRESENTATION(#8311,#8179);
#8092=PROPERTY_DEFINITION_REPRESENTATION(#8312,#8180);
#8093=PROPERTY_DEFINITION_REPRESENTATION(#8313,#8181);
#8094=PROPERTY_DEFINITION_REPRESENTATION(#8314,#8182);
#8095=PROPERTY_DEFINITION_REPRESENTATION(#8315,#8183);
#8096=PROPERTY_DEFINITION_REPRESENTATION(#8316,#8184);
#8097=PROPERTY_DEFINITION_REPRESENTATION(#8317,#8185);
#8098=PROPERTY_DEFINITION_REPRESENTATION(#8318,#8186);
#8099=PROPERTY_DEFINITION_REPRESENTATION(#8319,#8187);
#8100=PROPERTY_DEFINITION_REPRESENTATION(#8320,#8188);
#8101=PROPERTY_DEFINITION_REPRESENTATION(#8321,#8189);
#8102=PROPERTY_DEFINITION_REPRESENTATION(#8322,#8190);
#8103=PROPERTY_DEFINITION_REPRESENTATION(#8323,#8191);
#8104=PROPERTY_DEFINITION_REPRESENTATION(#8324,#8192);
#8105=PROPERTY_DEFINITION_REPRESENTATION(#8325,#8193);
#8106=PROPERTY_DEFINITION_REPRESENTATION(#8326,#8194);
#8107=PROPERTY_DEFINITION_REPRESENTATION(#8327,#8195);
#8108=PROPERTY_DEFINITION_REPRESENTATION(#8328,#8196);
#8109=PROPERTY_DEFINITION_REPRESENTATION(#8329,#8197);
#8110=PROPERTY_DEFINITION_REPRESENTATION(#8330,#8198);
#8111=PROPERTY_DEFINITION_REPRESENTATION(#8331,#8199);
#8112=PROPERTY_DEFINITION_REPRESENTATION(#8332,#8200);
#8113=PROPERTY_DEFINITION_REPRESENTATION(#8333,#8201);
#8114=PROPERTY_DEFINITION_REPRESENTATION(#8334,#8202);
#8115=PROPERTY_DEFINITION_REPRESENTATION(#8335,#8203);
#8116=PROPERTY_DEFINITION_REPRESENTATION(#8336,#8204);
#8117=PROPERTY_DEFINITION_REPRESENTATION(#8337,#8205);
#8118=PROPERTY_DEFINITION_REPRESENTATION(#8338,#8206);
#8119=PROPERTY_DEFINITION_REPRESENTATION(#8339,#8207);
#8120=PROPERTY_DEFINITION_REPRESENTATION(#8340,#8208);
#8121=PROPERTY_DEFINITION_REPRESENTATION(#8341,#8209);
#8122=PROPERTY_DEFINITION_REPRESENTATION(#8342,#8210);
#8123=PROPERTY_DEFINITION_REPRESENTATION(#8343,#8211);
#8124=PROPERTY_DEFINITION_REPRESENTATION(#8344,#8212);
#8125=PROPERTY_DEFINITION_REPRESENTATION(#8345,#8213);
#8126=PROPERTY_DEFINITION_REPRESENTATION(#8346,#8214);
#8127=PROPERTY_DEFINITION_REPRESENTATION(#8347,#8215);
#8128=PROPERTY_DEFINITION_REPRESENTATION(#8348,#8216);
#8129=PROPERTY_DEFINITION_REPRESENTATION(#8349,#8217);
#8130=PROPERTY_DEFINITION_REPRESENTATION(#8350,#8218);
#8131=PROPERTY_DEFINITION_REPRESENTATION(#8351,#8219);
#8132=PROPERTY_DEFINITION_REPRESENTATION(#8352,#8220);
#8133=PROPERTY_DEFINITION_REPRESENTATION(#8353,#8221);
#8134=PROPERTY_DEFINITION_REPRESENTATION(#8354,#8222);
#8135=PROPERTY_DEFINITION_REPRESENTATION(#8355,#8223);
#8136=PROPERTY_DEFINITION_REPRESENTATION(#8356,#8224);
#8137=PROPERTY_DEFINITION_REPRESENTATION(#8357,#8225);
#8138=PROPERTY_DEFINITION_REPRESENTATION(#8358,#8226);
#8139=PROPERTY_DEFINITION_REPRESENTATION(#8359,#8227);
#8140=PROPERTY_DEFINITION_REPRESENTATION(#8360,#8228);
#8141=PROPERTY_DEFINITION_REPRESENTATION(#8361,#8229);
#8142=PROPERTY_DEFINITION_REPRESENTATION(#8362,#8230);
#8143=PROPERTY_DEFINITION_REPRESENTATION(#8363,#8231);
#8144=PROPERTY_DEFINITION_REPRESENTATION(#8364,#8232);
#8145=PROPERTY_DEFINITION_REPRESENTATION(#8365,#8233);
#8146=PROPERTY_DEFINITION_REPRESENTATION(#8366,#8234);
#8147=PROPERTY_DEFINITION_REPRESENTATION(#8367,#8235);
#8148=PROPERTY_DEFINITION_REPRESENTATION(#8368,#8236);
#8149=PROPERTY_DEFINITION_REPRESENTATION(#8369,#8237);
#8150=PROPERTY_DEFINITION_REPRESENTATION(#8370,#8238);
#8151=PROPERTY_DEFINITION_REPRESENTATION(#8371,#8239);
#8152=PROPERTY_DEFINITION_REPRESENTATION(#8372,#8240);
#8153=PROPERTY_DEFINITION_REPRESENTATION(#8373,#8241);
#8154=PROPERTY_DEFINITION_REPRESENTATION(#8374,#8242);
#8155=PROPERTY_DEFINITION_REPRESENTATION(#8375,#8243);
#8156=PROPERTY_DEFINITION_REPRESENTATION(#8376,#8244);
#8157=PROPERTY_DEFINITION_REPRESENTATION(#8377,#8245);
#8158=PROPERTY_DEFINITION_REPRESENTATION(#8378,#8246);
#8159=PROPERTY_DEFINITION_REPRESENTATION(#8379,#8247);
#8160=PROPERTY_DEFINITION_REPRESENTATION(#8380,#8248);
#8161=PROPERTY_DEFINITION_REPRESENTATION(#8381,#8249);
#8162=PROPERTY_DEFINITION_REPRESENTATION(#8382,#8250);
#8163=PROPERTY_DEFINITION_REPRESENTATION(#8383,#8251);
#8164=REPRESENTATION('material name',(#8252),#14827);
#8165=REPRESENTATION('density',(#8032),#14827);
#8166=REPRESENTATION('material name',(#8253),#14828);
#8167=REPRESENTATION('density',(#8033),#14828);
#8168=REPRESENTATION('material name',(#8254),#14829);
#8169=REPRESENTATION('density',(#8034),#14829);
#8170=REPRESENTATION('material name',(#8255),#14830);
#8171=REPRESENTATION('density',(#8035),#14830);
#8172=REPRESENTATION('material name',(#8256),#14831);
#8173=REPRESENTATION('density',(#8036),#14831);
#8174=REPRESENTATION('material name',(#8257),#14832);
#8175=REPRESENTATION('density',(#8037),#14832);
#8176=REPRESENTATION('material name',(#8258),#14833);
#8177=REPRESENTATION('density',(#8038),#14833);
#8178=REPRESENTATION('material name',(#8259),#14834);
#8179=REPRESENTATION('density',(#8039),#14834);
#8180=REPRESENTATION('material name',(#8260),#14836);
#8181=REPRESENTATION('density',(#8040),#14836);
#8182=REPRESENTATION('material name',(#8261),#14837);
#8183=REPRESENTATION('density',(#8041),#14837);
#8184=REPRESENTATION('material name',(#8262),#14838);
#8185=REPRESENTATION('density',(#8042),#14838);
#8186=REPRESENTATION('material name',(#8263),#14839);
#8187=REPRESENTATION('density',(#8043),#14839);
#8188=REPRESENTATION('material name',(#8264),#14840);
#8189=REPRESENTATION('density',(#8044),#14840);
#8190=REPRESENTATION('material name',(#8265),#14842);
#8191=REPRESENTATION('density',(#8045),#14842);
#8192=REPRESENTATION('material name',(#8266),#14843);
#8193=REPRESENTATION('density',(#8046),#14843);
#8194=REPRESENTATION('material name',(#8267),#14844);
#8195=REPRESENTATION('density',(#8047),#14844);
#8196=REPRESENTATION('material name',(#8268),#14845);
#8197=REPRESENTATION('density',(#8048),#14845);
#8198=REPRESENTATION('material name',(#8269),#14846);
#8199=REPRESENTATION('density',(#8049),#14846);
#8200=REPRESENTATION('material name',(#8270),#14847);
#8201=REPRESENTATION('density',(#8050),#14847);
#8202=REPRESENTATION('material name',(#8271),#14848);
#8203=REPRESENTATION('density',(#8051),#14848);
#8204=REPRESENTATION('material name',(#8272),#14849);
#8205=REPRESENTATION('density',(#8052),#14849);
#8206=REPRESENTATION('material name',(#8273),#14850);
#8207=REPRESENTATION('density',(#8053),#14850);
#8208=REPRESENTATION('material name',(#8274),#14852);
#8209=REPRESENTATION('density',(#8054),#14852);
#8210=REPRESENTATION('material name',(#8275),#14853);
#8211=REPRESENTATION('density',(#8055),#14853);
#8212=REPRESENTATION('material name',(#8276),#14854);
#8213=REPRESENTATION('density',(#8056),#14854);
#8214=REPRESENTATION('material name',(#8277),#14855);
#8215=REPRESENTATION('density',(#8057),#14855);
#8216=REPRESENTATION('material name',(#8278),#14856);
#8217=REPRESENTATION('density',(#8058),#14856);
#8218=REPRESENTATION('material name',(#8279),#14857);
#8219=REPRESENTATION('density',(#8059),#14857);
#8220=REPRESENTATION('material name',(#8280),#14858);
#8221=REPRESENTATION('density',(#8060),#14858);
#8222=REPRESENTATION('material name',(#8281),#14859);
#8223=REPRESENTATION('density',(#8061),#14859);
#8224=REPRESENTATION('material name',(#8282),#14861);
#8225=REPRESENTATION('density',(#8062),#14861);
#8226=REPRESENTATION('material name',(#8283),#14863);
#8227=REPRESENTATION('density',(#8063),#14863);
#8228=REPRESENTATION('material name',(#8284),#14864);
#8229=REPRESENTATION('density',(#8064),#14864);
#8230=REPRESENTATION('material name',(#8285),#14865);
#8231=REPRESENTATION('density',(#8065),#14865);
#8232=REPRESENTATION('material name',(#8286),#14867);
#8233=REPRESENTATION('density',(#8066),#14867);
#8234=REPRESENTATION('material name',(#8287),#14868);
#8235=REPRESENTATION('density',(#8067),#14868);
#8236=REPRESENTATION('material name',(#8288),#14869);
#8237=REPRESENTATION('density',(#8068),#14869);
#8238=REPRESENTATION('material name',(#8289),#14870);
#8239=REPRESENTATION('density',(#8069),#14870);
#8240=REPRESENTATION('material name',(#8290),#14871);
#8241=REPRESENTATION('density',(#8070),#14871);
#8242=REPRESENTATION('material name',(#8291),#14873);
#8243=REPRESENTATION('density',(#8071),#14873);
#8244=REPRESENTATION('material name',(#8292),#14874);
#8245=REPRESENTATION('density',(#8072),#14874);
#8246=REPRESENTATION('material name',(#8293),#14875);
#8247=REPRESENTATION('density',(#8073),#14875);
#8248=REPRESENTATION('material name',(#8294),#14876);
#8249=REPRESENTATION('density',(#8074),#14876);
#8250=REPRESENTATION('material name',(#8295),#14877);
#8251=REPRESENTATION('density',(#8075),#14877);
#8252=DESCRIPTIVE_REPRESENTATION_ITEM('Steel','Steel');
#8253=DESCRIPTIVE_REPRESENTATION_ITEM('Steel','Steel');
#8254=DESCRIPTIVE_REPRESENTATION_ITEM('Steel','Steel');
#8255=DESCRIPTIVE_REPRESENTATION_ITEM('Steel','Steel');
#8256=DESCRIPTIVE_REPRESENTATION_ITEM('Steel','Steel');
#8257=DESCRIPTIVE_REPRESENTATION_ITEM('Steel','Steel');
#8258=DESCRIPTIVE_REPRESENTATION_ITEM('Steel','Steel');
#8259=DESCRIPTIVE_REPRESENTATION_ITEM('Steel','Steel');
#8260=DESCRIPTIVE_REPRESENTATION_ITEM('Steel','Steel');
#8261=DESCRIPTIVE_REPRESENTATION_ITEM('Steel','Steel');
#8262=DESCRIPTIVE_REPRESENTATION_ITEM('Steel','Steel');
#8263=DESCRIPTIVE_REPRESENTATION_ITEM('Steel','Steel');
#8264=DESCRIPTIVE_REPRESENTATION_ITEM('Steel','Steel');
#8265=DESCRIPTIVE_REPRESENTATION_ITEM('Steel','Steel');
#8266=DESCRIPTIVE_REPRESENTATION_ITEM('Steel','Steel');
#8267=DESCRIPTIVE_REPRESENTATION_ITEM('Steel','Steel');
#8268=DESCRIPTIVE_REPRESENTATION_ITEM('Steel','Steel');
#8269=DESCRIPTIVE_REPRESENTATION_ITEM('Steel','Steel');
#8270=DESCRIPTIVE_REPRESENTATION_ITEM('Steel','Steel');
#8271=DESCRIPTIVE_REPRESENTATION_ITEM('Steel','Steel');
#8272=DESCRIPTIVE_REPRESENTATION_ITEM('Steel','Steel');
#8273=DESCRIPTIVE_REPRESENTATION_ITEM('Steel','Steel');
#8274=DESCRIPTIVE_REPRESENTATION_ITEM('Steel','Steel');
#8275=DESCRIPTIVE_REPRESENTATION_ITEM('Steel','Steel');
#8276=DESCRIPTIVE_REPRESENTATION_ITEM('Steel','Steel');
#8277=DESCRIPTIVE_REPRESENTATION_ITEM('Steel','Steel');
#8278=DESCRIPTIVE_REPRESENTATION_ITEM('Steel','Steel');
#8279=DESCRIPTIVE_REPRESENTATION_ITEM('Steel','Steel');
#8280=DESCRIPTIVE_REPRESENTATION_ITEM('Steel','Steel');
#8281=DESCRIPTIVE_REPRESENTATION_ITEM('Steel','Steel');
#8282=DESCRIPTIVE_REPRESENTATION_ITEM('Steel','Steel');
#8283=DESCRIPTIVE_REPRESENTATION_ITEM('Steel','Steel');
#8284=DESCRIPTIVE_REPRESENTATION_ITEM('Steel','Steel');
#8285=DESCRIPTIVE_REPRESENTATION_ITEM('Steel','Steel');
#8286=DESCRIPTIVE_REPRESENTATION_ITEM('Steel','Steel');
#8287=DESCRIPTIVE_REPRESENTATION_ITEM('Steel','Steel');
#8288=DESCRIPTIVE_REPRESENTATION_ITEM('Steel','Steel');
#8289=DESCRIPTIVE_REPRESENTATION_ITEM('Steel','Steel');
#8290=DESCRIPTIVE_REPRESENTATION_ITEM('Steel','Steel');
#8291=DESCRIPTIVE_REPRESENTATION_ITEM('Steel','Steel');
#8292=DESCRIPTIVE_REPRESENTATION_ITEM('Steel','Steel');
#8293=DESCRIPTIVE_REPRESENTATION_ITEM('Steel','Steel');
#8294=DESCRIPTIVE_REPRESENTATION_ITEM('Steel','Steel');
#8295=DESCRIPTIVE_REPRESENTATION_ITEM('Steel','Steel');
#8296=PROPERTY_DEFINITION('material property','material name',#15124);
#8297=PROPERTY_DEFINITION('material property','density of part',#15124);
#8298=PROPERTY_DEFINITION('material property','material name',#15125);
#8299=PROPERTY_DEFINITION('material property','density of part',#15125);
#8300=PROPERTY_DEFINITION('material property','material name',#15126);
#8301=PROPERTY_DEFINITION('material property','density of part',#15126);
#8302=PROPERTY_DEFINITION('material property','material name',#15127);
#8303=PROPERTY_DEFINITION('material property','density of part',#15127);
#8304=PROPERTY_DEFINITION('material property','material name',#15128);
#8305=PROPERTY_DEFINITION('material property','density of part',#15128);
#8306=PROPERTY_DEFINITION('material property','material name',#15129);
#8307=PROPERTY_DEFINITION('material property','density of part',#15129);
#8308=PROPERTY_DEFINITION('material property','material name',#15130);
#8309=PROPERTY_DEFINITION('material property','density of part',#15130);
#8310=PROPERTY_DEFINITION('material property','material name',#15131);
#8311=PROPERTY_DEFINITION('material property','density of part',#15131);
#8312=PROPERTY_DEFINITION('material property','material name',#15133);
#8313=PROPERTY_DEFINITION('material property','density of part',#15133);
#8314=PROPERTY_DEFINITION('material property','material name',#15134);
#8315=PROPERTY_DEFINITION('material property','density of part',#15134);
#8316=PROPERTY_DEFINITION('material property','material name',#15135);
#8317=PROPERTY_DEFINITION('material property','density of part',#15135);
#8318=PROPERTY_DEFINITION('material property','material name',#15136);
#8319=PROPERTY_DEFINITION('material property','density of part',#15136);
#8320=PROPERTY_DEFINITION('material property','material name',#15137);
#8321=PROPERTY_DEFINITION('material property','density of part',#15137);
#8322=PROPERTY_DEFINITION('material property','material name',#15139);
#8323=PROPERTY_DEFINITION('material property','density of part',#15139);
#8324=PROPERTY_DEFINITION('material property','material name',#15140);
#8325=PROPERTY_DEFINITION('material property','density of part',#15140);
#8326=PROPERTY_DEFINITION('material property','material name',#15141);
#8327=PROPERTY_DEFINITION('material property','density of part',#15141);
#8328=PROPERTY_DEFINITION('material property','material name',#15142);
#8329=PROPERTY_DEFINITION('material property','density of part',#15142);
#8330=PROPERTY_DEFINITION('material property','material name',#15143);
#8331=PROPERTY_DEFINITION('material property','density of part',#15143);
#8332=PROPERTY_DEFINITION('material property','material name',#15144);
#8333=PROPERTY_DEFINITION('material property','density of part',#15144);
#8334=PROPERTY_DEFINITION('material property','material name',#15145);
#8335=PROPERTY_DEFINITION('material property','density of part',#15145);
#8336=PROPERTY_DEFINITION('material property','material name',#15146);
#8337=PROPERTY_DEFINITION('material property','density of part',#15146);
#8338=PROPERTY_DEFINITION('material property','material name',#15147);
#8339=PROPERTY_DEFINITION('material property','density of part',#15147);
#8340=PROPERTY_DEFINITION('material property','material name',#15149);
#8341=PROPERTY_DEFINITION('material property','density of part',#15149);
#8342=PROPERTY_DEFINITION('material property','material name',#15150);
#8343=PROPERTY_DEFINITION('material property','density of part',#15150);
#8344=PROPERTY_DEFINITION('material property','material name',#15151);
#8345=PROPERTY_DEFINITION('material property','density of part',#15151);
#8346=PROPERTY_DEFINITION('material property','material name',#15152);
#8347=PROPERTY_DEFINITION('material property','density of part',#15152);
#8348=PROPERTY_DEFINITION('material property','material name',#15153);
#8349=PROPERTY_DEFINITION('material property','density of part',#15153);
#8350=PROPERTY_DEFINITION('material property','material name',#15154);
#8351=PROPERTY_DEFINITION('material property','density of part',#15154);
#8352=PROPERTY_DEFINITION('material property','material name',#15155);
#8353=PROPERTY_DEFINITION('material property','density of part',#15155);
#8354=PROPERTY_DEFINITION('material property','material name',#15156);
#8355=PROPERTY_DEFINITION('material property','density of part',#15156);
#8356=PROPERTY_DEFINITION('material property','material name',#15158);
#8357=PROPERTY_DEFINITION('material property','density of part',#15158);
#8358=PROPERTY_DEFINITION('material property','material name',#15160);
#8359=PROPERTY_DEFINITION('material property','density of part',#15160);
#8360=PROPERTY_DEFINITION('material property','material name',#15161);
#8361=PROPERTY_DEFINITION('material property','density of part',#15161);
#8362=PROPERTY_DEFINITION('material property','material name',#15162);
#8363=PROPERTY_DEFINITION('material property','density of part',#15162);
#8364=PROPERTY_DEFINITION('material property','material name',#15164);
#8365=PROPERTY_DEFINITION('material property','density of part',#15164);
#8366=PROPERTY_DEFINITION('material property','material name',#15165);
#8367=PROPERTY_DEFINITION('material property','density of part',#15165);
#8368=PROPERTY_DEFINITION('material property','material name',#15166);
#8369=PROPERTY_DEFINITION('material property','density of part',#15166);
#8370=PROPERTY_DEFINITION('material property','material name',#15167);
#8371=PROPERTY_DEFINITION('material property','density of part',#15167);
#8372=PROPERTY_DEFINITION('material property','material name',#15168);
#8373=PROPERTY_DEFINITION('material property','density of part',#15168);
#8374=PROPERTY_DEFINITION('material property','material name',#15170);
#8375=PROPERTY_DEFINITION('material property','density of part',#15170);
#8376=PROPERTY_DEFINITION('material property','material name',#15171);
#8377=PROPERTY_DEFINITION('material property','density of part',#15171);
#8378=PROPERTY_DEFINITION('material property','material name',#15172);
#8379=PROPERTY_DEFINITION('material property','density of part',#15172);
#8380=PROPERTY_DEFINITION('material property','material name',#15173);
#8381=PROPERTY_DEFINITION('material property','density of part',#15173);
#8382=PROPERTY_DEFINITION('material property','material name',#15174);
#8383=PROPERTY_DEFINITION('material property','density of part',#15174);
#8384=AXIS2_PLACEMENT_3D('',#11946,#9397,#9398);
#8385=AXIS2_PLACEMENT_3D('',#11947,#9399,#9400);
#8386=AXIS2_PLACEMENT_3D('',#11948,#9401,#9402);
#8387=AXIS2_PLACEMENT_3D('',#11949,#9403,#9404);
#8388=AXIS2_PLACEMENT_3D('',#11951,#9405,#9406);
#8389=AXIS2_PLACEMENT_3D('',#11954,#9408,#9409);
#8390=AXIS2_PLACEMENT_3D('',#11955,#9410,#9411);
#8391=AXIS2_PLACEMENT_3D('',#11957,#9412,#9413);
#8392=AXIS2_PLACEMENT_3D('',#11960,#9415,#9416);
#8393=AXIS2_PLACEMENT_3D('',#11961,#9417,#9418);
#8394=AXIS2_PLACEMENT_3D('',#11963,#9419,#9420);
#8395=AXIS2_PLACEMENT_3D('',#11966,#9422,#9423);
#8396=AXIS2_PLACEMENT_3D('',#11967,#9424,#9425);
#8397=AXIS2_PLACEMENT_3D('',#11969,#9426,#9427);
#8398=AXIS2_PLACEMENT_3D('',#11972,#9429,#9430);
#8399=AXIS2_PLACEMENT_3D('',#11973,#9431,#9432);
#8400=AXIS2_PLACEMENT_3D('',#11975,#9433,#9434);
#8401=AXIS2_PLACEMENT_3D('',#11978,#9436,#9437);
#8402=AXIS2_PLACEMENT_3D('',#11979,#9438,#9439);
#8403=AXIS2_PLACEMENT_3D('',#11981,#9440,#9441);
#8404=AXIS2_PLACEMENT_3D('',#11984,#9443,#9444);
#8405=AXIS2_PLACEMENT_3D('',#11985,#9445,#9446);
#8406=AXIS2_PLACEMENT_3D('',#11987,#9447,#9448);
#8407=AXIS2_PLACEMENT_3D('',#11990,#9450,#9451);
#8408=AXIS2_PLACEMENT_3D('',#11991,#9452,#9453);
#8409=AXIS2_PLACEMENT_3D('',#11993,#9454,#9455);
#8410=AXIS2_PLACEMENT_3D('',#11996,#9457,#9458);
#8411=AXIS2_PLACEMENT_3D('',#11997,#9459,#9460);
#8412=AXIS2_PLACEMENT_3D('',#11999,#9461,#9462);
#8413=AXIS2_PLACEMENT_3D('',#12002,#9464,#9465);
#8414=AXIS2_PLACEMENT_3D('',#12003,#9466,#9467);
#8415=AXIS2_PLACEMENT_3D('',#12005,#9468,#9469);
#8416=AXIS2_PLACEMENT_3D('',#12008,#9471,#9472);
#8417=AXIS2_PLACEMENT_3D('',#12009,#9473,#9474);
#8418=AXIS2_PLACEMENT_3D('',#12011,#9475,#9476);
#8419=AXIS2_PLACEMENT_3D('',#12014,#9478,#9479);
#8420=AXIS2_PLACEMENT_3D('',#12015,#9480,#9481);
#8421=AXIS2_PLACEMENT_3D('',#12017,#9482,#9483);
#8422=AXIS2_PLACEMENT_3D('',#12020,#9485,#9486);
#8423=AXIS2_PLACEMENT_3D('',#12021,#9487,#9488);
#8424=AXIS2_PLACEMENT_3D('',#12030,#9493,#9494);
#8425=AXIS2_PLACEMENT_3D('',#12036,#9498,#9499);
#8426=AXIS2_PLACEMENT_3D('',#12042,#9503,#9504);
#8427=AXIS2_PLACEMENT_3D('',#12045,#9507,#9508);
#8428=AXIS2_PLACEMENT_3D('',#12046,#9509,#9510);
#8429=AXIS2_PLACEMENT_3D('',#12047,#9511,#9512);
#8430=AXIS2_PLACEMENT_3D('',#12048,#9513,#9514);
#8431=AXIS2_PLACEMENT_3D('',#12057,#9519,#9520);
#8432=AXIS2_PLACEMENT_3D('',#12063,#9524,#9525);
#8433=AXIS2_PLACEMENT_3D('',#12069,#9529,#9530);
#8434=AXIS2_PLACEMENT_3D('',#12072,#9533,#9534);
#8435=AXIS2_PLACEMENT_3D('',#12073,#9535,#9536);
#8436=AXIS2_PLACEMENT_3D('',#12074,#9537,#9538);
#8437=AXIS2_PLACEMENT_3D('',#12075,#9539,#9540);
#8438=AXIS2_PLACEMENT_3D('',#12084,#9545,#9546);
#8439=AXIS2_PLACEMENT_3D('',#12090,#9550,#9551);
#8440=AXIS2_PLACEMENT_3D('',#12096,#9555,#9556);
#8441=AXIS2_PLACEMENT_3D('',#12099,#9559,#9560);
#8442=AXIS2_PLACEMENT_3D('',#12100,#9561,#9562);
#8443=AXIS2_PLACEMENT_3D('',#12101,#9563,#9564);
#8444=AXIS2_PLACEMENT_3D('',#12102,#9565,#9566);
#8445=AXIS2_PLACEMENT_3D('',#12180,#9568,#9569);
#8446=AXIS2_PLACEMENT_3D('',#12182,#9570,#9571);
#8447=AXIS2_PLACEMENT_3D('',#12185,#9573,#9574);
#8448=AXIS2_PLACEMENT_3D('',#12186,#9575,#9576);
#8449=AXIS2_PLACEMENT_3D('',#12187,#9577,#9578);
#8450=AXIS2_PLACEMENT_3D('',#12189,#9579,#9580);
#8451=AXIS2_PLACEMENT_3D('',#12192,#9582,#9583);
#8452=AXIS2_PLACEMENT_3D('',#12193,#9584,#9585);
#8453=AXIS2_PLACEMENT_3D('',#12194,#9586,#9587);
#8454=AXIS2_PLACEMENT_3D('',#12196,#9588,#9589);
#8455=AXIS2_PLACEMENT_3D('',#12199,#9591,#9592);
#8456=AXIS2_PLACEMENT_3D('',#12200,#9593,#9594);
#8457=AXIS2_PLACEMENT_3D('',#12201,#9595,#9596);
#8458=AXIS2_PLACEMENT_3D('',#12203,#9597,#9598);
#8459=AXIS2_PLACEMENT_3D('',#12206,#9600,#9601);
#8460=AXIS2_PLACEMENT_3D('',#12207,#9602,#9603);
#8461=AXIS2_PLACEMENT_3D('',#12208,#9604,#9605);
#8462=AXIS2_PLACEMENT_3D('',#12213,#9607,#9608);
#8463=AXIS2_PLACEMENT_3D('',#12216,#9610,#9611);
#8464=AXIS2_PLACEMENT_3D('',#12217,#9612,#9613);
#8465=AXIS2_PLACEMENT_3D('',#12218,#9614,#9615);
#8466=AXIS2_PLACEMENT_3D('',#12219,#9616,#9617);
#8467=AXIS2_PLACEMENT_3D('',#12224,#9619,#9620);
#8468=AXIS2_PLACEMENT_3D('',#12227,#9622,#9623);
#8469=AXIS2_PLACEMENT_3D('',#12228,#9624,#9625);
#8470=AXIS2_PLACEMENT_3D('',#12229,#9626,#9627);
#8471=AXIS2_PLACEMENT_3D('',#12230,#9628,#9629);
#8472=AXIS2_PLACEMENT_3D('',#12235,#9631,#9632);
#8473=AXIS2_PLACEMENT_3D('',#12238,#9634,#9635);
#8474=AXIS2_PLACEMENT_3D('',#12239,#9636,#9637);
#8475=AXIS2_PLACEMENT_3D('',#12240,#9638,#9639);
#8476=AXIS2_PLACEMENT_3D('',#12241,#9640,#9641);
#8477=AXIS2_PLACEMENT_3D('',#12246,#9643,#9644);
#8478=AXIS2_PLACEMENT_3D('',#12249,#9646,#9647);
#8479=AXIS2_PLACEMENT_3D('',#12250,#9648,#9649);
#8480=AXIS2_PLACEMENT_3D('',#12251,#9650,#9651);
#8481=AXIS2_PLACEMENT_3D('',#12252,#9652,#9653);
#8482=AXIS2_PLACEMENT_3D('',#12254,#9654,#9655);
#8483=AXIS2_PLACEMENT_3D('',#12256,#9656,#9657);
#8484=AXIS2_PLACEMENT_3D('',#12257,#9658,#9659);
#8485=AXIS2_PLACEMENT_3D('',#12258,#9660,#9661);
#8486=AXIS2_PLACEMENT_3D('',#12259,#9662,#9663);
#8487=AXIS2_PLACEMENT_3D('',#12260,#9664,#9665);
#8488=AXIS2_PLACEMENT_3D('',#12262,#9666,#9667);
#8489=AXIS2_PLACEMENT_3D('',#12264,#9668,#9669);
#8490=AXIS2_PLACEMENT_3D('',#12266,#9670,#9671);
#8491=AXIS2_PLACEMENT_3D('',#12268,#9672,#9673);
#8492=AXIS2_PLACEMENT_3D('',#12269,#9674,#9675);
#8493=AXIS2_PLACEMENT_3D('',#12271,#9676,#9677);
#8494=AXIS2_PLACEMENT_3D('',#12273,#9679,#9680);
#8495=AXIS2_PLACEMENT_3D('',#12275,#9681,#9682);
#8496=AXIS2_PLACEMENT_3D('',#12277,#9684,#9685);
#8497=AXIS2_PLACEMENT_3D('',#12279,#9686,#9687);
#8498=AXIS2_PLACEMENT_3D('',#12281,#9689,#9690);
#8499=AXIS2_PLACEMENT_3D('',#12283,#9691,#9692);
#8500=AXIS2_PLACEMENT_3D('',#12285,#9694,#9695);
#8501=AXIS2_PLACEMENT_3D('',#12287,#9696,#9697);
#8502=AXIS2_PLACEMENT_3D('',#12289,#9699,#9700);
#8503=AXIS2_PLACEMENT_3D('',#12291,#9701,#9702);
#8504=AXIS2_PLACEMENT_3D('',#12294,#9704,#9705);
#8505=AXIS2_PLACEMENT_3D('',#12295,#9706,#9707);
#8506=AXIS2_PLACEMENT_3D('',#12297,#9708,#9709);
#8507=AXIS2_PLACEMENT_3D('',#12298,#9710,#9711);
#8508=AXIS2_PLACEMENT_3D('',#12301,#9713,#9714);
#8509=AXIS2_PLACEMENT_3D('',#12302,#9715,#9716);
#8510=AXIS2_PLACEMENT_3D('',#12305,#9718,#9719);
#8511=AXIS2_PLACEMENT_3D('',#12306,#9720,#9721);
#8512=AXIS2_PLACEMENT_3D('',#12307,#9722,#9723);
#8513=AXIS2_PLACEMENT_3D('',#12308,#9724,#9725);
#8514=AXIS2_PLACEMENT_3D('',#12309,#9726,#9727);
#8515=AXIS2_PLACEMENT_3D('',#12311,#9728,#9729);
#8516=AXIS2_PLACEMENT_3D('',#12314,#9731,#9732);
#8517=AXIS2_PLACEMENT_3D('',#12315,#9733,#9734);
#8518=AXIS2_PLACEMENT_3D('',#12317,#9735,#9736);
#8519=AXIS2_PLACEMENT_3D('',#12318,#9737,#9738);
#8520=AXIS2_PLACEMENT_3D('',#12320,#9739,#9740);
#8521=AXIS2_PLACEMENT_3D('',#12323,#9742,#9743);
#8522=AXIS2_PLACEMENT_3D('',#12324,#9744,#9745);
#8523=AXIS2_PLACEMENT_3D('',#12326,#9746,#9747);
#8524=AXIS2_PLACEMENT_3D('',#12327,#9748,#9749);
#8525=AXIS2_PLACEMENT_3D('',#12329,#9750,#9751);
#8526=AXIS2_PLACEMENT_3D('',#12332,#9753,#9754);
#8527=AXIS2_PLACEMENT_3D('',#12333,#9755,#9756);
#8528=AXIS2_PLACEMENT_3D('',#12335,#9757,#9758);
#8529=AXIS2_PLACEMENT_3D('',#12336,#9759,#9760);
#8530=AXIS2_PLACEMENT_3D('',#12338,#9761,#9762);
#8531=AXIS2_PLACEMENT_3D('',#12341,#9764,#9765);
#8532=AXIS2_PLACEMENT_3D('',#12342,#9766,#9767);
#8533=AXIS2_PLACEMENT_3D('',#12344,#9768,#9769);
#8534=AXIS2_PLACEMENT_3D('',#12345,#9770,#9771);
#8535=AXIS2_PLACEMENT_3D('',#12347,#9772,#9773);
#8536=AXIS2_PLACEMENT_3D('',#12349,#9775,#9776);
#8537=AXIS2_PLACEMENT_3D('',#12351,#9777,#9778);
#8538=AXIS2_PLACEMENT_3D('',#12353,#9780,#9781);
#8539=AXIS2_PLACEMENT_3D('',#12355,#9782,#9783);
#8540=AXIS2_PLACEMENT_3D('',#12357,#9785,#9786);
#8541=AXIS2_PLACEMENT_3D('',#12359,#9787,#9788);
#8542=AXIS2_PLACEMENT_3D('',#12361,#9790,#9791);
#8543=AXIS2_PLACEMENT_3D('',#12363,#9792,#9793);
#8544=AXIS2_PLACEMENT_3D('',#12366,#9795,#9796);
#8545=AXIS2_PLACEMENT_3D('',#12367,#9797,#9798);
#8546=AXIS2_PLACEMENT_3D('',#12369,#9799,#9800);
#8547=AXIS2_PLACEMENT_3D('',#12370,#9801,#9802);
#8548=AXIS2_PLACEMENT_3D('',#12372,#9803,#9804);
#8549=AXIS2_PLACEMENT_3D('',#12374,#9806,#9807);
#8550=AXIS2_PLACEMENT_3D('',#12376,#9808,#9809);
#8551=AXIS2_PLACEMENT_3D('',#12379,#9811,#9812);
#8552=AXIS2_PLACEMENT_3D('',#12380,#9813,#9814);
#8553=AXIS2_PLACEMENT_3D('',#12381,#9815,#9816);
#8554=AXIS2_PLACEMENT_3D('',#12382,#9817,#9818);
#8555=AXIS2_PLACEMENT_3D('',#12383,#9819,#9820);
#8556=AXIS2_PLACEMENT_3D('',#12461,#9822,#9823);
#8557=AXIS2_PLACEMENT_3D('',#12463,#9824,#9825);
#8558=AXIS2_PLACEMENT_3D('',#12466,#9827,#9828);
#8559=AXIS2_PLACEMENT_3D('',#12467,#9829,#9830);
#8560=AXIS2_PLACEMENT_3D('',#12468,#9831,#9832);
#8561=AXIS2_PLACEMENT_3D('',#12470,#9833,#9834);
#8562=AXIS2_PLACEMENT_3D('',#12473,#9836,#9837);
#8563=AXIS2_PLACEMENT_3D('',#12474,#9838,#9839);
#8564=AXIS2_PLACEMENT_3D('',#12475,#9840,#9841);
#8565=AXIS2_PLACEMENT_3D('',#12477,#9842,#9843);
#8566=AXIS2_PLACEMENT_3D('',#12480,#9845,#9846);
#8567=AXIS2_PLACEMENT_3D('',#12481,#9847,#9848);
#8568=AXIS2_PLACEMENT_3D('',#12482,#9849,#9850);
#8569=AXIS2_PLACEMENT_3D('',#12484,#9851,#9852);
#8570=AXIS2_PLACEMENT_3D('',#12487,#9854,#9855);
#8571=AXIS2_PLACEMENT_3D('',#12488,#9856,#9857);
#8572=AXIS2_PLACEMENT_3D('',#12489,#9858,#9859);
#8573=AXIS2_PLACEMENT_3D('',#12494,#9861,#9862);
#8574=AXIS2_PLACEMENT_3D('',#12497,#9864,#9865);
#8575=AXIS2_PLACEMENT_3D('',#12498,#9866,#9867);
#8576=AXIS2_PLACEMENT_3D('',#12499,#9868,#9869);
#8577=AXIS2_PLACEMENT_3D('',#12500,#9870,#9871);
#8578=AXIS2_PLACEMENT_3D('',#12505,#9873,#9874);
#8579=AXIS2_PLACEMENT_3D('',#12508,#9876,#9877);
#8580=AXIS2_PLACEMENT_3D('',#12509,#9878,#9879);
#8581=AXIS2_PLACEMENT_3D('',#12510,#9880,#9881);
#8582=AXIS2_PLACEMENT_3D('',#12511,#9882,#9883);
#8583=AXIS2_PLACEMENT_3D('',#12516,#9885,#9886);
#8584=AXIS2_PLACEMENT_3D('',#12519,#9888,#9889);
#8585=AXIS2_PLACEMENT_3D('',#12520,#9890,#9891);
#8586=AXIS2_PLACEMENT_3D('',#12521,#9892,#9893);
#8587=AXIS2_PLACEMENT_3D('',#12522,#9894,#9895);
#8588=AXIS2_PLACEMENT_3D('',#12527,#9897,#9898);
#8589=AXIS2_PLACEMENT_3D('',#12530,#9900,#9901);
#8590=AXIS2_PLACEMENT_3D('',#12531,#9902,#9903);
#8591=AXIS2_PLACEMENT_3D('',#12532,#9904,#9905);
#8592=AXIS2_PLACEMENT_3D('',#12533,#9906,#9907);
#8593=AXIS2_PLACEMENT_3D('',#12535,#9908,#9909);
#8594=AXIS2_PLACEMENT_3D('',#12537,#9910,#9911);
#8595=AXIS2_PLACEMENT_3D('',#12538,#9912,#9913);
#8596=AXIS2_PLACEMENT_3D('',#12539,#9914,#9915);
#8597=AXIS2_PLACEMENT_3D('',#12540,#9916,#9917);
#8598=AXIS2_PLACEMENT_3D('',#12541,#9918,#9919);
#8599=AXIS2_PLACEMENT_3D('',#12543,#9920,#9921);
#8600=AXIS2_PLACEMENT_3D('',#12545,#9922,#9923);
#8601=AXIS2_PLACEMENT_3D('',#12547,#9924,#9925);
#8602=AXIS2_PLACEMENT_3D('',#12549,#9926,#9927);
#8603=AXIS2_PLACEMENT_3D('',#12550,#9928,#9929);
#8604=AXIS2_PLACEMENT_3D('',#12552,#9930,#9931);
#8605=AXIS2_PLACEMENT_3D('',#12554,#9933,#9934);
#8606=AXIS2_PLACEMENT_3D('',#12556,#9935,#9936);
#8607=AXIS2_PLACEMENT_3D('',#12558,#9938,#9939);
#8608=AXIS2_PLACEMENT_3D('',#12560,#9940,#9941);
#8609=AXIS2_PLACEMENT_3D('',#12562,#9943,#9944);
#8610=AXIS2_PLACEMENT_3D('',#12564,#9945,#9946);
#8611=AXIS2_PLACEMENT_3D('',#12566,#9948,#9949);
#8612=AXIS2_PLACEMENT_3D('',#12568,#9950,#9951);
#8613=AXIS2_PLACEMENT_3D('',#12570,#9953,#9954);
#8614=AXIS2_PLACEMENT_3D('',#12572,#9955,#9956);
#8615=AXIS2_PLACEMENT_3D('',#12575,#9958,#9959);
#8616=AXIS2_PLACEMENT_3D('',#12576,#9960,#9961);
#8617=AXIS2_PLACEMENT_3D('',#12578,#9962,#9963);
#8618=AXIS2_PLACEMENT_3D('',#12579,#9964,#9965);
#8619=AXIS2_PLACEMENT_3D('',#12582,#9967,#9968);
#8620=AXIS2_PLACEMENT_3D('',#12583,#9969,#9970);
#8621=AXIS2_PLACEMENT_3D('',#12586,#9972,#9973);
#8622=AXIS2_PLACEMENT_3D('',#12587,#9974,#9975);
#8623=AXIS2_PLACEMENT_3D('',#12588,#9976,#9977);
#8624=AXIS2_PLACEMENT_3D('',#12589,#9978,#9979);
#8625=AXIS2_PLACEMENT_3D('',#12590,#9980,#9981);
#8626=AXIS2_PLACEMENT_3D('',#12592,#9982,#9983);
#8627=AXIS2_PLACEMENT_3D('',#12595,#9985,#9986);
#8628=AXIS2_PLACEMENT_3D('',#12596,#9987,#9988);
#8629=AXIS2_PLACEMENT_3D('',#12598,#9989,#9990);
#8630=AXIS2_PLACEMENT_3D('',#12599,#9991,#9992);
#8631=AXIS2_PLACEMENT_3D('',#12601,#9993,#9994);
#8632=AXIS2_PLACEMENT_3D('',#12604,#9996,#9997);
#8633=AXIS2_PLACEMENT_3D('',#12605,#9998,#9999);
#8634=AXIS2_PLACEMENT_3D('',#12607,#10000,#10001);
#8635=AXIS2_PLACEMENT_3D('',#12608,#10002,#10003);
#8636=AXIS2_PLACEMENT_3D('',#12610,#10004,#10005);
#8637=AXIS2_PLACEMENT_3D('',#12613,#10007,#10008);
#8638=AXIS2_PLACEMENT_3D('',#12614,#10009,#10010);
#8639=AXIS2_PLACEMENT_3D('',#12616,#10011,#10012);
#8640=AXIS2_PLACEMENT_3D('',#12617,#10013,#10014);
#8641=AXIS2_PLACEMENT_3D('',#12619,#10015,#10016);
#8642=AXIS2_PLACEMENT_3D('',#12622,#10018,#10019);
#8643=AXIS2_PLACEMENT_3D('',#12623,#10020,#10021);
#8644=AXIS2_PLACEMENT_3D('',#12625,#10022,#10023);
#8645=AXIS2_PLACEMENT_3D('',#12626,#10024,#10025);
#8646=AXIS2_PLACEMENT_3D('',#12628,#10026,#10027);
#8647=AXIS2_PLACEMENT_3D('',#12630,#10029,#10030);
#8648=AXIS2_PLACEMENT_3D('',#12632,#10031,#10032);
#8649=AXIS2_PLACEMENT_3D('',#12634,#10034,#10035);
#8650=AXIS2_PLACEMENT_3D('',#12636,#10036,#10037);
#8651=AXIS2_PLACEMENT_3D('',#12638,#10039,#10040);
#8652=AXIS2_PLACEMENT_3D('',#12640,#10041,#10042);
#8653=AXIS2_PLACEMENT_3D('',#12642,#10044,#10045);
#8654=AXIS2_PLACEMENT_3D('',#12644,#10046,#10047);
#8655=AXIS2_PLACEMENT_3D('',#12647,#10049,#10050);
#8656=AXIS2_PLACEMENT_3D('',#12648,#10051,#10052);
#8657=AXIS2_PLACEMENT_3D('',#12650,#10053,#10054);
#8658=AXIS2_PLACEMENT_3D('',#12651,#10055,#10056);
#8659=AXIS2_PLACEMENT_3D('',#12653,#10057,#10058);
#8660=AXIS2_PLACEMENT_3D('',#12655,#10060,#10061);
#8661=AXIS2_PLACEMENT_3D('',#12657,#10062,#10063);
#8662=AXIS2_PLACEMENT_3D('',#12660,#10065,#10066);
#8663=AXIS2_PLACEMENT_3D('',#12661,#10067,#10068);
#8664=AXIS2_PLACEMENT_3D('',#12662,#10069,#10070);
#8665=AXIS2_PLACEMENT_3D('',#12663,#10071,#10072);
#8666=AXIS2_PLACEMENT_3D('',#12664,#10073,#10074);
#8667=AXIS2_PLACEMENT_3D('',#12666,#10075,#10076);
#8668=AXIS2_PLACEMENT_3D('',#12669,#10078,#10079);
#8669=AXIS2_PLACEMENT_3D('',#12670,#10080,#10081);
#8670=AXIS2_PLACEMENT_3D('',#12672,#10082,#10083);
#8671=AXIS2_PLACEMENT_3D('',#12673,#10084,#10085);
#8672=AXIS2_PLACEMENT_3D('',#12675,#10086,#10087);
#8673=AXIS2_PLACEMENT_3D('',#12678,#10089,#10090);
#8674=AXIS2_PLACEMENT_3D('',#12679,#10091,#10092);
#8675=AXIS2_PLACEMENT_3D('',#12681,#10093,#10094);
#8676=AXIS2_PLACEMENT_3D('',#12682,#10095,#10096);
#8677=AXIS2_PLACEMENT_3D('',#12684,#10097,#10098);
#8678=AXIS2_PLACEMENT_3D('',#12687,#10100,#10101);
#8679=AXIS2_PLACEMENT_3D('',#12688,#10102,#10103);
#8680=AXIS2_PLACEMENT_3D('',#12690,#10104,#10105);
#8681=AXIS2_PLACEMENT_3D('',#12691,#10106,#10107);
#8682=AXIS2_PLACEMENT_3D('',#12693,#10108,#10109);
#8683=AXIS2_PLACEMENT_3D('',#12696,#10111,#10112);
#8684=AXIS2_PLACEMENT_3D('',#12697,#10113,#10114);
#8685=AXIS2_PLACEMENT_3D('',#12699,#10115,#10116);
#8686=AXIS2_PLACEMENT_3D('',#12700,#10117,#10118);
#8687=AXIS2_PLACEMENT_3D('',#12702,#10119,#10120);
#8688=AXIS2_PLACEMENT_3D('',#12704,#10122,#10123);
#8689=AXIS2_PLACEMENT_3D('',#12706,#10124,#10125);
#8690=AXIS2_PLACEMENT_3D('',#12708,#10127,#10128);
#8691=AXIS2_PLACEMENT_3D('',#12710,#10129,#10130);
#8692=AXIS2_PLACEMENT_3D('',#12712,#10132,#10133);
#8693=AXIS2_PLACEMENT_3D('',#12714,#10134,#10135);
#8694=AXIS2_PLACEMENT_3D('',#12716,#10137,#10138);
#8695=AXIS2_PLACEMENT_3D('',#12725,#10143,#10144);
#8696=AXIS2_PLACEMENT_3D('',#12731,#10148,#10149);
#8697=AXIS2_PLACEMENT_3D('',#12737,#10153,#10154);
#8698=AXIS2_PLACEMENT_3D('',#12743,#10158,#10159);
#8699=AXIS2_PLACEMENT_3D('',#12749,#10163,#10164);
#8700=AXIS2_PLACEMENT_3D('',#12755,#10168,#10169);
#8701=AXIS2_PLACEMENT_3D('',#12761,#10173,#10174);
#8702=AXIS2_PLACEMENT_3D('',#12767,#10178,#10179);
#8703=AXIS2_PLACEMENT_3D('',#12773,#10183,#10184);
#8704=AXIS2_PLACEMENT_3D('',#12779,#10188,#10189);
#8705=AXIS2_PLACEMENT_3D('',#12785,#10193,#10194);
#8706=AXIS2_PLACEMENT_3D('',#12788,#10197,#10198);
#8707=AXIS2_PLACEMENT_3D('',#12789,#10199,#10200);
#8708=AXIS2_PLACEMENT_3D('',#12790,#10201,#10202);
#8709=AXIS2_PLACEMENT_3D('',#12791,#10203,#10204);
#8710=AXIS2_PLACEMENT_3D('',#12792,#10205,#10206);
#8711=AXIS2_PLACEMENT_3D('',#12795,#10207,#10208);
#8712=AXIS2_PLACEMENT_3D('',#12796,#10209,#10210);
#8713=AXIS2_PLACEMENT_3D('',#12798,#10211,#10212);
#8714=AXIS2_PLACEMENT_3D('',#12800,#10213,#10214);
#8715=AXIS2_PLACEMENT_3D('',#12801,#10215,#10216);
#8716=AXIS2_PLACEMENT_3D('',#12802,#10217,#10218);
#8717=AXIS2_PLACEMENT_3D('',#12805,#10220,#10221);
#8718=AXIS2_PLACEMENT_3D('',#12806,#10222,#10223);
#8719=AXIS2_PLACEMENT_3D('',#12808,#10224,#10225);
#8720=AXIS2_PLACEMENT_3D('',#12811,#10227,#10228);
#8721=AXIS2_PLACEMENT_3D('',#12812,#10229,#10230);
#8722=AXIS2_PLACEMENT_3D('',#12815,#10232,#10233);
#8723=AXIS2_PLACEMENT_3D('',#12816,#10234,#10235);
#8724=AXIS2_PLACEMENT_3D('',#12817,#10236,#10237);
#8725=AXIS2_PLACEMENT_3D('',#12819,#10238,#10239);
#8726=AXIS2_PLACEMENT_3D('',#12821,#10241,#10242);
#8727=AXIS2_PLACEMENT_3D('',#12823,#10243,#10244);
#8728=AXIS2_PLACEMENT_3D('',#12824,#10245,#10246);
#8729=AXIS2_PLACEMENT_3D('',#12826,#10248,#10249);
#8730=AXIS2_PLACEMENT_3D('',#12827,#10250,#10251);
#8731=AXIS2_PLACEMENT_3D('',#12830,#10252,#10253);
#8732=AXIS2_PLACEMENT_3D('',#12831,#10254,#10255);
#8733=AXIS2_PLACEMENT_3D('',#12833,#10256,#10257);
#8734=AXIS2_PLACEMENT_3D('',#12835,#10258,#10259);
#8735=AXIS2_PLACEMENT_3D('',#12836,#10260,#10261);
#8736=AXIS2_PLACEMENT_3D('',#12837,#10262,#10263);
#8737=AXIS2_PLACEMENT_3D('',#12839,#10264,#10265);
#8738=AXIS2_PLACEMENT_3D('',#12841,#10267,#10268);
#8739=AXIS2_PLACEMENT_3D('',#12843,#10269,#10270);
#8740=AXIS2_PLACEMENT_3D('',#12845,#10271,#10272);
#8741=AXIS2_PLACEMENT_3D('',#12846,#10273,#10274);
#8742=AXIS2_PLACEMENT_3D('',#12848,#10275,#10276);
#8743=AXIS2_PLACEMENT_3D('',#12850,#10278,#10279);
#8744=AXIS2_PLACEMENT_3D('',#12852,#10280,#10281);
#8745=AXIS2_PLACEMENT_3D('',#12854,#10283,#10284);
#8746=AXIS2_PLACEMENT_3D('',#12856,#10285,#10286);
#8747=AXIS2_PLACEMENT_3D('',#12858,#10288,#10289);
#8748=AXIS2_PLACEMENT_3D('',#12859,#10290,#10291);
#8749=AXIS2_PLACEMENT_3D('',#12861,#10293,#10294);
#8750=AXIS2_PLACEMENT_3D('',#12862,#10295,#10296);
#8751=AXIS2_PLACEMENT_3D('',#12865,#10297,#10298);
#8752=AXIS2_PLACEMENT_3D('',#12866,#10299,#10300);
#8753=AXIS2_PLACEMENT_3D('',#12869,#10301,#10302);
#8754=AXIS2_PLACEMENT_3D('',#12870,#10303,#10304);
#8755=AXIS2_PLACEMENT_3D('',#12873,#10305,#10306);
#8756=AXIS2_PLACEMENT_3D('',#12874,#10307,#10308);
#8757=AXIS2_PLACEMENT_3D('',#12877,#10309,#10310);
#8758=AXIS2_PLACEMENT_3D('',#12878,#10311,#10312);
#8759=AXIS2_PLACEMENT_3D('',#12881,#10313,#10314);
#8760=AXIS2_PLACEMENT_3D('',#12882,#10315,#10316);
#8761=AXIS2_PLACEMENT_3D('',#12885,#10317,#10318);
#8762=AXIS2_PLACEMENT_3D('',#12886,#10319,#10320);
#8763=AXIS2_PLACEMENT_3D('',#12889,#10321,#10322);
#8764=AXIS2_PLACEMENT_3D('',#12890,#10323,#10324);
#8765=AXIS2_PLACEMENT_3D('',#12893,#10325,#10326);
#8766=AXIS2_PLACEMENT_3D('',#12894,#10327,#10328);
#8767=AXIS2_PLACEMENT_3D('',#12895,#10329,#10330);
#8768=AXIS2_PLACEMENT_3D('',#12921,#10331,#10332);
#8769=AXIS2_PLACEMENT_3D('',#12945,#10333,#10334);
#8770=AXIS2_PLACEMENT_3D('',#12946,#10335,#10336);
#8771=AXIS2_PLACEMENT_3D('',#12948,#10337,#10338);
#8772=AXIS2_PLACEMENT_3D('',#12973,#10339,#10340);
#8773=AXIS2_PLACEMENT_3D('',#12998,#10341,#10342);
#8774=AXIS2_PLACEMENT_3D('',#13014,#10344,#10345);
#8775=AXIS2_PLACEMENT_3D('',#13029,#10346,#10347);
#8776=AXIS2_PLACEMENT_3D('',#13054,#10348,#10349);
#8777=AXIS2_PLACEMENT_3D('',#13079,#10350,#10351);
#8778=AXIS2_PLACEMENT_3D('',#13104,#10352,#10353);
#8779=AXIS2_PLACEMENT_3D('',#13128,#10354,#10355);
#8780=AXIS2_PLACEMENT_3D('',#13129,#10356,#10357);
#8781=AXIS2_PLACEMENT_3D('',#13131,#10358,#10359);
#8782=AXIS2_PLACEMENT_3D('',#13132,#10360,#10361);
#8783=AXIS2_PLACEMENT_3D('',#13133,#10362,#10363);
#8784=AXIS2_PLACEMENT_3D('',#13157,#10364,#10365);
#8785=AXIS2_PLACEMENT_3D('',#13158,#10366,#10367);
#8786=AXIS2_PLACEMENT_3D('',#13160,#10368,#10369);
#8787=AXIS2_PLACEMENT_3D('',#13161,#10370,#10371);
#8788=AXIS2_PLACEMENT_3D('',#13162,#10372,#10373);
#8789=AXIS2_PLACEMENT_3D('',#13186,#10374,#10375);
#8790=AXIS2_PLACEMENT_3D('',#13187,#10376,#10377);
#8791=AXIS2_PLACEMENT_3D('',#13189,#10378,#10379);
#8792=AXIS2_PLACEMENT_3D('',#13190,#10380,#10381);
#8793=AXIS2_PLACEMENT_3D('',#13191,#10382,#10383);
#8794=AXIS2_PLACEMENT_3D('',#13206,#10384,#10385);
#8795=AXIS2_PLACEMENT_3D('',#13219,#10386,#10387);
#8796=AXIS2_PLACEMENT_3D('',#13221,#10388,#10389);
#8797=AXIS2_PLACEMENT_3D('',#13222,#10390,#10391);
#8798=AXIS2_PLACEMENT_3D('',#13223,#10392,#10393);
#8799=AXIS2_PLACEMENT_3D('',#13247,#10394,#10395);
#8800=AXIS2_PLACEMENT_3D('',#13248,#10396,#10397);
#8801=AXIS2_PLACEMENT_3D('',#13250,#10398,#10399);
#8802=AXIS2_PLACEMENT_3D('',#13251,#10400,#10401);
#8803=AXIS2_PLACEMENT_3D('',#13252,#10402,#10403);
#8804=AXIS2_PLACEMENT_3D('',#13276,#10404,#10405);
#8805=AXIS2_PLACEMENT_3D('',#13277,#10406,#10407);
#8806=AXIS2_PLACEMENT_3D('',#13279,#10408,#10409);
#8807=AXIS2_PLACEMENT_3D('',#13280,#10410,#10411);
#8808=AXIS2_PLACEMENT_3D('',#13281,#10412,#10413);
#8809=AXIS2_PLACEMENT_3D('',#13305,#10414,#10415);
#8810=AXIS2_PLACEMENT_3D('',#13306,#10416,#10417);
#8811=AXIS2_PLACEMENT_3D('',#13308,#10418,#10419);
#8812=AXIS2_PLACEMENT_3D('',#13311,#10421,#10422);
#8813=AXIS2_PLACEMENT_3D('',#13335,#10423,#10424);
#8814=AXIS2_PLACEMENT_3D('',#13336,#10425,#10426);
#8815=AXIS2_PLACEMENT_3D('',#13337,#10427,#10428);
#8816=AXIS2_PLACEMENT_3D('',#13338,#10429,#10430);
#8817=AXIS2_PLACEMENT_3D('',#13339,#10431,#10432);
#8818=AXIS2_PLACEMENT_3D('',#13340,#10433,#10434);
#8819=AXIS2_PLACEMENT_3D('',#13341,#10435,#10436);
#8820=AXIS2_PLACEMENT_3D('',#13342,#10437,#10438);
#8821=AXIS2_PLACEMENT_3D('',#13343,#10439,#10440);
#8822=AXIS2_PLACEMENT_3D('',#13345,#10441,#10442);
#8823=AXIS2_PLACEMENT_3D('',#13347,#10443,#10444);
#8824=AXIS2_PLACEMENT_3D('',#13348,#10445,#10446);
#8825=AXIS2_PLACEMENT_3D('',#13350,#10447,#10448);
#8826=AXIS2_PLACEMENT_3D('',#13352,#10450,#10451);
#8827=AXIS2_PLACEMENT_3D('',#13354,#10452,#10453);
#8828=AXIS2_PLACEMENT_3D('',#13355,#10454,#10455);
#8829=AXIS2_PLACEMENT_3D('',#13357,#10457,#10458);
#8830=AXIS2_PLACEMENT_3D('',#13359,#10459,#10460);
#8831=AXIS2_PLACEMENT_3D('',#13361,#10461,#10462);
#8832=AXIS2_PLACEMENT_3D('',#13362,#10463,#10464);
#8833=AXIS2_PLACEMENT_3D('',#13364,#10465,#10466);
#8834=AXIS2_PLACEMENT_3D('',#13366,#10468,#10469);
#8835=AXIS2_PLACEMENT_3D('',#13368,#10470,#10471);
#8836=AXIS2_PLACEMENT_3D('',#13369,#10472,#10473);
#8837=AXIS2_PLACEMENT_3D('',#13371,#10475,#10476);
#8838=AXIS2_PLACEMENT_3D('',#13372,#10477,#10478);
#8839=AXIS2_PLACEMENT_3D('',#13373,#10479,#10480);
#8840=AXIS2_PLACEMENT_3D('',#13374,#10481,#10482);
#8841=AXIS2_PLACEMENT_3D('',#13375,#10483,#10484);
#8842=AXIS2_PLACEMENT_3D('',#13376,#10485,#10486);
#8843=AXIS2_PLACEMENT_3D('',#13377,#10487,#10488);
#8844=AXIS2_PLACEMENT_3D('',#13378,#10489,#10490);
#8845=AXIS2_PLACEMENT_3D('',#13380,#10491,#10492);
#8846=AXIS2_PLACEMENT_3D('',#13383,#10494,#10495);
#8847=AXIS2_PLACEMENT_3D('',#13384,#10496,#10497);
#8848=AXIS2_PLACEMENT_3D('',#13389,#10499,#10500);
#8849=AXIS2_PLACEMENT_3D('',#13392,#10502,#10503);
#8850=AXIS2_PLACEMENT_3D('',#13393,#10504,#10505);
#8851=AXIS2_PLACEMENT_3D('',#13399,#10509,#10510);
#8852=AXIS2_PLACEMENT_3D('',#13403,#10512,#10513);
#8853=AXIS2_PLACEMENT_3D('',#13407,#10515,#10516);
#8854=AXIS2_PLACEMENT_3D('',#13410,#10518,#10519);
#8855=AXIS2_PLACEMENT_3D('',#13412,#10520,#10521);
#8856=AXIS2_PLACEMENT_3D('',#13414,#10522,#10523);
#8857=AXIS2_PLACEMENT_3D('',#13415,#10524,#10525);
#8858=AXIS2_PLACEMENT_3D('',#13419,#10528,#10529);
#8859=AXIS2_PLACEMENT_3D('',#13421,#10530,#10531);
#8860=AXIS2_PLACEMENT_3D('',#13423,#10533,#10534);
#8861=AXIS2_PLACEMENT_3D('',#13426,#10536,#10537);
#8862=AXIS2_PLACEMENT_3D('',#13427,#10538,#10539);
#8863=AXIS2_PLACEMENT_3D('',#13432,#10542,#10543);
#8864=AXIS2_PLACEMENT_3D('',#13433,#10544,#10545);
#8865=AXIS2_PLACEMENT_3D('',#13437,#10548,#10549);
#8866=AXIS2_PLACEMENT_3D('',#13438,#10550,#10551);
#8867=AXIS2_PLACEMENT_3D('',#13440,#10553,#10554);
#8868=AXIS2_PLACEMENT_3D('',#13441,#10555,#10556);
#8869=AXIS2_PLACEMENT_3D('',#13442,#10557,#10558);
#8870=AXIS2_PLACEMENT_3D('',#13444,#10559,#10560);
#8871=AXIS2_PLACEMENT_3D('',#13446,#10561,#10562);
#8872=AXIS2_PLACEMENT_3D('',#13447,#10563,#10564);
#8873=AXIS2_PLACEMENT_3D('',#13449,#10566,#10567);
#8874=AXIS2_PLACEMENT_3D('',#13452,#10569,#10570);
#8875=AXIS2_PLACEMENT_3D('',#13453,#10571,#10572);
#8876=AXIS2_PLACEMENT_3D('',#13454,#10573,#10574);
#8877=AXIS2_PLACEMENT_3D('',#13455,#10575,#10576);
#8878=AXIS2_PLACEMENT_3D('',#13457,#10577,#10578);
#8879=AXIS2_PLACEMENT_3D('',#13460,#10580,#10581);
#8880=AXIS2_PLACEMENT_3D('',#13461,#10582,#10583);
#8881=AXIS2_PLACEMENT_3D('',#13462,#10584,#10585);
#8882=AXIS2_PLACEMENT_3D('',#13464,#10586,#10587);
#8883=AXIS2_PLACEMENT_3D('',#13467,#10589,#10590);
#8884=AXIS2_PLACEMENT_3D('',#13468,#10591,#10592);
#8885=AXIS2_PLACEMENT_3D('',#13469,#10593,#10594);
#8886=AXIS2_PLACEMENT_3D('',#13470,#10595,#10596);
#8887=AXIS2_PLACEMENT_3D('',#13471,#10597,#10598);
#8888=AXIS2_PLACEMENT_3D('',#13473,#10599,#10600);
#8889=AXIS2_PLACEMENT_3D('',#13476,#10602,#10603);
#8890=AXIS2_PLACEMENT_3D('',#13477,#10604,#10605);
#8891=AXIS2_PLACEMENT_3D('',#13479,#10606,#10607);
#8892=AXIS2_PLACEMENT_3D('',#13482,#10609,#10610);
#8893=AXIS2_PLACEMENT_3D('',#13483,#10611,#10612);
#8894=AXIS2_PLACEMENT_3D('',#13484,#10613,#10614);
#8895=AXIS2_PLACEMENT_3D('',#13485,#10615,#10616);
#8896=AXIS2_PLACEMENT_3D('',#13486,#10617,#10618);
#8897=AXIS2_PLACEMENT_3D('',#13490,#10620,#10621);
#8898=AXIS2_PLACEMENT_3D('',#13491,#10622,#10623);
#8899=AXIS2_PLACEMENT_3D('',#13508,#10624,#10625);
#8900=AXIS2_PLACEMENT_3D('',#13565,#10627,#10628);
#8901=AXIS2_PLACEMENT_3D('',#13567,#10630,#10631);
#8902=AXIS2_PLACEMENT_3D('',#13569,#10632,#10633);
#8903=AXIS2_PLACEMENT_3D('',#13572,#10635,#10636);
#8904=AXIS2_PLACEMENT_3D('',#13573,#10637,#10638);
#8905=AXIS2_PLACEMENT_3D('',#13575,#10639,#10640);
#8906=AXIS2_PLACEMENT_3D('',#13578,#10642,#10643);
#8907=AXIS2_PLACEMENT_3D('',#13579,#10644,#10645);
#8908=AXIS2_PLACEMENT_3D('',#13580,#10646,#10647);
#8909=AXIS2_PLACEMENT_3D('',#13581,#10648,#10649);
#8910=AXIS2_PLACEMENT_3D('',#13582,#10650,#10651);
#8911=AXIS2_PLACEMENT_3D('',#13584,#10652,#10653);
#8912=AXIS2_PLACEMENT_3D('',#13587,#10655,#10656);
#8913=AXIS2_PLACEMENT_3D('',#13588,#10657,#10658);
#8914=AXIS2_PLACEMENT_3D('',#13589,#10659,#10660);
#8915=AXIS2_PLACEMENT_3D('',#13591,#10661,#10662);
#8916=AXIS2_PLACEMENT_3D('',#13593,#10663,#10664);
#8917=AXIS2_PLACEMENT_3D('',#13594,#10665,#10666);
#8918=AXIS2_PLACEMENT_3D('',#13596,#10667,#10668);
#8919=AXIS2_PLACEMENT_3D('',#13598,#10669,#10670);
#8920=AXIS2_PLACEMENT_3D('',#13599,#10671,#10672);
#8921=AXIS2_PLACEMENT_3D('',#13601,#10674,#10675);
#8922=AXIS2_PLACEMENT_3D('',#13604,#10677,#10678);
#8923=AXIS2_PLACEMENT_3D('',#13605,#10679,#10680);
#8924=AXIS2_PLACEMENT_3D('',#13607,#10681,#10682);
#8925=AXIS2_PLACEMENT_3D('',#13609,#10684,#10685);
#8926=AXIS2_PLACEMENT_3D('',#13610,#10686,#10687);
#8927=AXIS2_PLACEMENT_3D('',#13611,#10688,#10689);
#8928=AXIS2_PLACEMENT_3D('',#13612,#10690,#10691);
#8929=AXIS2_PLACEMENT_3D('',#13614,#10692,#10693);
#8930=AXIS2_PLACEMENT_3D('',#13617,#10695,#10696);
#8931=AXIS2_PLACEMENT_3D('',#13618,#10697,#10698);
#8932=AXIS2_PLACEMENT_3D('',#13620,#10699,#10700);
#8933=AXIS2_PLACEMENT_3D('',#13623,#10702,#10703);
#8934=AXIS2_PLACEMENT_3D('',#13624,#10704,#10705);
#8935=AXIS2_PLACEMENT_3D('',#13625,#10706,#10707);
#8936=AXIS2_PLACEMENT_3D('',#13626,#10708,#10709);
#8937=AXIS2_PLACEMENT_3D('',#13627,#10710,#10711);
#8938=AXIS2_PLACEMENT_3D('',#13629,#10712,#10713);
#8939=AXIS2_PLACEMENT_3D('',#13632,#10715,#10716);
#8940=AXIS2_PLACEMENT_3D('',#13633,#10717,#10718);
#8941=AXIS2_PLACEMENT_3D('',#13635,#10719,#10720);
#8942=AXIS2_PLACEMENT_3D('',#13638,#10722,#10723);
#8943=AXIS2_PLACEMENT_3D('',#13639,#10724,#10725);
#8944=AXIS2_PLACEMENT_3D('',#13640,#10726,#10727);
#8945=AXIS2_PLACEMENT_3D('',#13641,#10728,#10729);
#8946=AXIS2_PLACEMENT_3D('',#13642,#10730,#10731);
#8947=AXIS2_PLACEMENT_3D('',#13644,#10732,#10733);
#8948=AXIS2_PLACEMENT_3D('',#13647,#10735,#10736);
#8949=AXIS2_PLACEMENT_3D('',#13648,#10737,#10738);
#8950=AXIS2_PLACEMENT_3D('',#13650,#10739,#10740);
#8951=AXIS2_PLACEMENT_3D('',#13653,#10742,#10743);
#8952=AXIS2_PLACEMENT_3D('',#13654,#10744,#10745);
#8953=AXIS2_PLACEMENT_3D('',#13655,#10746,#10747);
#8954=AXIS2_PLACEMENT_3D('',#13656,#10748,#10749);
#8955=AXIS2_PLACEMENT_3D('',#13657,#10750,#10751);
#8956=AXIS2_PLACEMENT_3D('',#13659,#10752,#10753);
#8957=AXIS2_PLACEMENT_3D('',#13660,#10754,#10755);
#8958=AXIS2_PLACEMENT_3D('',#13662,#10756,#10757);
#8959=AXIS2_PLACEMENT_3D('',#13664,#10759,#10760);
#8960=AXIS2_PLACEMENT_3D('',#13666,#10761,#10762);
#8961=AXIS2_PLACEMENT_3D('',#13668,#10764,#10765);
#8962=AXIS2_PLACEMENT_3D('',#13670,#10766,#10767);
#8963=AXIS2_PLACEMENT_3D('',#13672,#10769,#10770);
#8964=AXIS2_PLACEMENT_3D('',#13674,#10771,#10772);
#8965=AXIS2_PLACEMENT_3D('',#13675,#10773,#10774);
#8966=AXIS2_PLACEMENT_3D('',#13677,#10775,#10776);
#8967=AXIS2_PLACEMENT_3D('',#13679,#10778,#10779);
#8968=AXIS2_PLACEMENT_3D('',#13681,#10780,#10781);
#8969=AXIS2_PLACEMENT_3D('',#13683,#10783,#10784);
#8970=AXIS2_PLACEMENT_3D('',#13685,#10785,#10786);
#8971=AXIS2_PLACEMENT_3D('',#13687,#10788,#10789);
#8972=AXIS2_PLACEMENT_3D('',#13688,#10790,#10791);
#8973=AXIS2_PLACEMENT_3D('',#13697,#10796,#10797);
#8974=AXIS2_PLACEMENT_3D('',#13703,#10801,#10802);
#8975=AXIS2_PLACEMENT_3D('',#13709,#10806,#10807);
#8976=AXIS2_PLACEMENT_3D('',#13715,#10811,#10812);
#8977=AXIS2_PLACEMENT_3D('',#13721,#10816,#10817);
#8978=AXIS2_PLACEMENT_3D('',#13724,#10820,#10821);
#8979=AXIS2_PLACEMENT_3D('',#13725,#10822,#10823);
#8980=AXIS2_PLACEMENT_3D('',#13726,#10824,#10825);
#8981=AXIS2_PLACEMENT_3D('',#13727,#10826,#10827);
#8982=AXIS2_PLACEMENT_3D('',#13728,#10828,#10829);
#8983=AXIS2_PLACEMENT_3D('',#13730,#10830,#10831);
#8984=AXIS2_PLACEMENT_3D('',#13733,#10833,#10834);
#8985=AXIS2_PLACEMENT_3D('',#13734,#10835,#10836);
#8986=AXIS2_PLACEMENT_3D('',#13743,#10841,#10842);
#8987=AXIS2_PLACEMENT_3D('',#13749,#10846,#10847);
#8988=AXIS2_PLACEMENT_3D('',#13755,#10851,#10852);
#8989=AXIS2_PLACEMENT_3D('',#13758,#10855,#10856);
#8990=AXIS2_PLACEMENT_3D('',#13763,#10858,#10859);
#8991=AXIS2_PLACEMENT_3D('',#13766,#10861,#10862);
#8992=AXIS2_PLACEMENT_3D('',#13767,#10863,#10864);
#8993=AXIS2_PLACEMENT_3D('',#13771,#10866,#10867);
#8994=AXIS2_PLACEMENT_3D('',#13774,#10869,#10870);
#8995=AXIS2_PLACEMENT_3D('',#13775,#10871,#10872);
#8996=AXIS2_PLACEMENT_3D('',#13779,#10875,#10876);
#8997=AXIS2_PLACEMENT_3D('',#13783,#10879,#10880);
#8998=AXIS2_PLACEMENT_3D('',#13784,#10881,#10882);
#8999=AXIS2_PLACEMENT_3D('',#13785,#10883,#10884);
#9000=AXIS2_PLACEMENT_3D('',#13787,#10885,#10886);
#9001=AXIS2_PLACEMENT_3D('',#13789,#10887,#10888);
#9002=AXIS2_PLACEMENT_3D('',#13790,#10889,#10890);
#9003=AXIS2_PLACEMENT_3D('',#13792,#10892,#10893);
#9004=AXIS2_PLACEMENT_3D('',#13795,#10895,#10896);
#9005=AXIS2_PLACEMENT_3D('',#13796,#10897,#10898);
#9006=AXIS2_PLACEMENT_3D('',#13797,#10899,#10900);
#9007=AXIS2_PLACEMENT_3D('',#13798,#10901,#10902);
#9008=AXIS2_PLACEMENT_3D('',#13799,#10903,#10904);
#9009=AXIS2_PLACEMENT_3D('',#13801,#10905,#10906);
#9010=AXIS2_PLACEMENT_3D('',#13804,#10908,#10909);
#9011=AXIS2_PLACEMENT_3D('',#13805,#10910,#10911);
#9012=AXIS2_PLACEMENT_3D('',#13807,#10912,#10913);
#9013=AXIS2_PLACEMENT_3D('',#13810,#10915,#10916);
#9014=AXIS2_PLACEMENT_3D('',#13811,#10917,#10918);
#9015=AXIS2_PLACEMENT_3D('',#13812,#10919,#10920);
#9016=AXIS2_PLACEMENT_3D('',#13813,#10921,#10922);
#9017=AXIS2_PLACEMENT_3D('',#13814,#10923,#10924);
#9018=AXIS2_PLACEMENT_3D('',#13818,#10926,#10927);
#9019=AXIS2_PLACEMENT_3D('',#13819,#10928,#10929);
#9020=AXIS2_PLACEMENT_3D('',#13836,#10930,#10931);
#9021=AXIS2_PLACEMENT_3D('',#13893,#10933,#10934);
#9022=AXIS2_PLACEMENT_3D('',#13895,#10936,#10937);
#9023=AXIS2_PLACEMENT_3D('',#13897,#10938,#10939);
#9024=AXIS2_PLACEMENT_3D('',#13900,#10941,#10942);
#9025=AXIS2_PLACEMENT_3D('',#13901,#10943,#10944);
#9026=AXIS2_PLACEMENT_3D('',#13903,#10945,#10946);
#9027=AXIS2_PLACEMENT_3D('',#13906,#10948,#10949);
#9028=AXIS2_PLACEMENT_3D('',#13907,#10950,#10951);
#9029=AXIS2_PLACEMENT_3D('',#13908,#10952,#10953);
#9030=AXIS2_PLACEMENT_3D('',#13909,#10954,#10955);
#9031=AXIS2_PLACEMENT_3D('',#13910,#10956,#10957);
#9032=AXIS2_PLACEMENT_3D('',#13912,#10958,#10959);
#9033=AXIS2_PLACEMENT_3D('',#13915,#10961,#10962);
#9034=AXIS2_PLACEMENT_3D('',#13916,#10963,#10964);
#9035=AXIS2_PLACEMENT_3D('',#13917,#10965,#10966);
#9036=AXIS2_PLACEMENT_3D('',#13919,#10967,#10968);
#9037=AXIS2_PLACEMENT_3D('',#13921,#10969,#10970);
#9038=AXIS2_PLACEMENT_3D('',#13922,#10971,#10972);
#9039=AXIS2_PLACEMENT_3D('',#13924,#10973,#10974);
#9040=AXIS2_PLACEMENT_3D('',#13926,#10975,#10976);
#9041=AXIS2_PLACEMENT_3D('',#13927,#10977,#10978);
#9042=AXIS2_PLACEMENT_3D('',#13929,#10980,#10981);
#9043=AXIS2_PLACEMENT_3D('',#13932,#10983,#10984);
#9044=AXIS2_PLACEMENT_3D('',#13933,#10985,#10986);
#9045=AXIS2_PLACEMENT_3D('',#13935,#10987,#10988);
#9046=AXIS2_PLACEMENT_3D('',#13937,#10990,#10991);
#9047=AXIS2_PLACEMENT_3D('',#13938,#10992,#10993);
#9048=AXIS2_PLACEMENT_3D('',#13939,#10994,#10995);
#9049=AXIS2_PLACEMENT_3D('',#13940,#10996,#10997);
#9050=AXIS2_PLACEMENT_3D('',#13942,#10998,#10999);
#9051=AXIS2_PLACEMENT_3D('',#13945,#11001,#11002);
#9052=AXIS2_PLACEMENT_3D('',#13946,#11003,#11004);
#9053=AXIS2_PLACEMENT_3D('',#13948,#11005,#11006);
#9054=AXIS2_PLACEMENT_3D('',#13951,#11008,#11009);
#9055=AXIS2_PLACEMENT_3D('',#13952,#11010,#11011);
#9056=AXIS2_PLACEMENT_3D('',#13953,#11012,#11013);
#9057=AXIS2_PLACEMENT_3D('',#13954,#11014,#11015);
#9058=AXIS2_PLACEMENT_3D('',#13955,#11016,#11017);
#9059=AXIS2_PLACEMENT_3D('',#13957,#11018,#11019);
#9060=AXIS2_PLACEMENT_3D('',#13960,#11021,#11022);
#9061=AXIS2_PLACEMENT_3D('',#13961,#11023,#11024);
#9062=AXIS2_PLACEMENT_3D('',#13963,#11025,#11026);
#9063=AXIS2_PLACEMENT_3D('',#13966,#11028,#11029);
#9064=AXIS2_PLACEMENT_3D('',#13967,#11030,#11031);
#9065=AXIS2_PLACEMENT_3D('',#13968,#11032,#11033);
#9066=AXIS2_PLACEMENT_3D('',#13969,#11034,#11035);
#9067=AXIS2_PLACEMENT_3D('',#13970,#11036,#11037);
#9068=AXIS2_PLACEMENT_3D('',#13972,#11038,#11039);
#9069=AXIS2_PLACEMENT_3D('',#13975,#11041,#11042);
#9070=AXIS2_PLACEMENT_3D('',#13976,#11043,#11044);
#9071=AXIS2_PLACEMENT_3D('',#13978,#11045,#11046);
#9072=AXIS2_PLACEMENT_3D('',#13981,#11048,#11049);
#9073=AXIS2_PLACEMENT_3D('',#13982,#11050,#11051);
#9074=AXIS2_PLACEMENT_3D('',#13983,#11052,#11053);
#9075=AXIS2_PLACEMENT_3D('',#13984,#11054,#11055);
#9076=AXIS2_PLACEMENT_3D('',#13985,#11056,#11057);
#9077=AXIS2_PLACEMENT_3D('',#13987,#11058,#11059);
#9078=AXIS2_PLACEMENT_3D('',#13988,#11060,#11061);
#9079=AXIS2_PLACEMENT_3D('',#13997,#11066,#11067);
#9080=AXIS2_PLACEMENT_3D('',#14003,#11071,#11072);
#9081=AXIS2_PLACEMENT_3D('',#14009,#11076,#11077);
#9082=AXIS2_PLACEMENT_3D('',#14015,#11081,#11082);
#9083=AXIS2_PLACEMENT_3D('',#14021,#11086,#11087);
#9084=AXIS2_PLACEMENT_3D('',#14024,#11090,#11091);
#9085=AXIS2_PLACEMENT_3D('',#14025,#11092,#11093);
#9086=AXIS2_PLACEMENT_3D('',#14027,#11094,#11095);
#9087=AXIS2_PLACEMENT_3D('',#14028,#11096,#11097);
#9088=AXIS2_PLACEMENT_3D('',#14030,#11098,#11099);
#9089=AXIS2_PLACEMENT_3D('',#14032,#11101,#11102);
#9090=AXIS2_PLACEMENT_3D('',#14034,#11104,#11105);
#9091=AXIS2_PLACEMENT_3D('',#14035,#11106,#11107);
#9092=AXIS2_PLACEMENT_3D('',#14036,#11108,#11109);
#9093=AXIS2_PLACEMENT_3D('',#14038,#11110,#11111);
#9094=AXIS2_PLACEMENT_3D('',#14041,#11113,#11114);
#9095=AXIS2_PLACEMENT_3D('',#14042,#11115,#11116);
#9096=AXIS2_PLACEMENT_3D('',#14051,#11121,#11122);
#9097=AXIS2_PLACEMENT_3D('',#14060,#11127,#11128);
#9098=AXIS2_PLACEMENT_3D('',#14066,#11132,#11133);
#9099=AXIS2_PLACEMENT_3D('',#14072,#11137,#11138);
#9100=AXIS2_PLACEMENT_3D('',#14075,#11141,#11142);
#9101=AXIS2_PLACEMENT_3D('',#14084,#11147,#11148);
#9102=AXIS2_PLACEMENT_3D('',#14093,#11153,#11154);
#9103=AXIS2_PLACEMENT_3D('',#14099,#11158,#11159);
#9104=AXIS2_PLACEMENT_3D('',#14105,#11163,#11164);
#9105=AXIS2_PLACEMENT_3D('',#14108,#11167,#11168);
#9106=AXIS2_PLACEMENT_3D('',#14111,#11171,#11172);
#9107=AXIS2_PLACEMENT_3D('',#14113,#11174,#11175);
#9108=AXIS2_PLACEMENT_3D('',#14115,#11177,#11178);
#9109=AXIS2_PLACEMENT_3D('',#14116,#11179,#11180);
#9110=AXIS2_PLACEMENT_3D('',#14117,#11181,#11182);
#9111=AXIS2_PLACEMENT_3D('',#14118,#11183,#11184);
#9112=AXIS2_PLACEMENT_3D('',#14119,#11185,#11186);
#9113=AXIS2_PLACEMENT_3D('',#14121,#11187,#11188);
#9114=AXIS2_PLACEMENT_3D('',#14124,#11190,#11191);
#9115=AXIS2_PLACEMENT_3D('',#14125,#11192,#11193);
#9116=AXIS2_PLACEMENT_3D('',#14127,#11194,#11195);
#9117=AXIS2_PLACEMENT_3D('',#14130,#11197,#11198);
#9118=AXIS2_PLACEMENT_3D('',#14131,#11199,#11200);
#9119=AXIS2_PLACEMENT_3D('',#14136,#11202,#11203);
#9120=AXIS2_PLACEMENT_3D('',#14139,#11205,#11206);
#9121=AXIS2_PLACEMENT_3D('',#14140,#11207,#11208);
#9122=AXIS2_PLACEMENT_3D('',#14146,#11212,#11213);
#9123=AXIS2_PLACEMENT_3D('',#14149,#11215,#11216);
#9124=AXIS2_PLACEMENT_3D('',#14150,#11217,#11218);
#9125=AXIS2_PLACEMENT_3D('',#14154,#11221,#11222);
#9126=AXIS2_PLACEMENT_3D('',#14155,#11223,#11224);
#9127=AXIS2_PLACEMENT_3D('',#14156,#11225,#11226);
#9128=AXIS2_PLACEMENT_3D('',#14157,#11227,#11228);
#9129=AXIS2_PLACEMENT_3D('',#14158,#11229,#11230);
#9130=AXIS2_PLACEMENT_3D('',#14160,#11231,#11232);
#9131=AXIS2_PLACEMENT_3D('',#14163,#11234,#11235);
#9132=AXIS2_PLACEMENT_3D('',#14164,#11236,#11237);
#9133=AXIS2_PLACEMENT_3D('',#14166,#11238,#11239);
#9134=AXIS2_PLACEMENT_3D('',#14169,#11241,#11242);
#9135=AXIS2_PLACEMENT_3D('',#14170,#11243,#11244);
#9136=AXIS2_PLACEMENT_3D('',#14171,#11245,#11246);
#9137=AXIS2_PLACEMENT_3D('',#14172,#11247,#11248);
#9138=AXIS2_PLACEMENT_3D('',#14173,#11249,#11250);
#9139=AXIS2_PLACEMENT_3D('',#14175,#11251,#11252);
#9140=AXIS2_PLACEMENT_3D('',#14178,#11254,#11255);
#9141=AXIS2_PLACEMENT_3D('',#14179,#11256,#11257);
#9142=AXIS2_PLACEMENT_3D('',#14181,#11258,#11259);
#9143=AXIS2_PLACEMENT_3D('',#14184,#11261,#11262);
#9144=AXIS2_PLACEMENT_3D('',#14185,#11263,#11264);
#9145=AXIS2_PLACEMENT_3D('',#14186,#11265,#11266);
#9146=AXIS2_PLACEMENT_3D('',#14187,#11267,#11268);
#9147=AXIS2_PLACEMENT_3D('',#14188,#11269,#11270);
#9148=AXIS2_PLACEMENT_3D('',#14189,#11271,#11272);
#9149=AXIS2_PLACEMENT_3D('',#14190,#11273,#11274);
#9150=AXIS2_PLACEMENT_3D('',#14191,#11275,#11276);
#9151=AXIS2_PLACEMENT_3D('',#14192,#11277,#11278);
#9152=AXIS2_PLACEMENT_3D('',#14194,#11279,#11280);
#9153=AXIS2_PLACEMENT_3D('',#14197,#11282,#11283);
#9154=AXIS2_PLACEMENT_3D('',#14198,#11284,#11285);
#9155=AXIS2_PLACEMENT_3D('',#14200,#11286,#11287);
#9156=AXIS2_PLACEMENT_3D('',#14203,#11289,#11290);
#9157=AXIS2_PLACEMENT_3D('',#14204,#11291,#11292);
#9158=AXIS2_PLACEMENT_3D('',#14206,#11293,#11294);
#9159=AXIS2_PLACEMENT_3D('',#14209,#11296,#11297);
#9160=AXIS2_PLACEMENT_3D('',#14210,#11298,#11299);
#9161=AXIS2_PLACEMENT_3D('',#14212,#11300,#11301);
#9162=AXIS2_PLACEMENT_3D('',#14215,#11303,#11304);
#9163=AXIS2_PLACEMENT_3D('',#14216,#11305,#11306);
#9164=AXIS2_PLACEMENT_3D('',#14218,#11307,#11308);
#9165=AXIS2_PLACEMENT_3D('',#14221,#11310,#11311);
#9166=AXIS2_PLACEMENT_3D('',#14222,#11312,#11313);
#9167=AXIS2_PLACEMENT_3D('',#14231,#11318,#11319);
#9168=AXIS2_PLACEMENT_3D('',#14237,#11323,#11324);
#9169=AXIS2_PLACEMENT_3D('',#14243,#11328,#11329);
#9170=AXIS2_PLACEMENT_3D('',#14246,#11332,#11333);
#9171=AXIS2_PLACEMENT_3D('',#14247,#11334,#11335);
#9172=AXIS2_PLACEMENT_3D('',#14248,#11336,#11337);
#9173=AXIS2_PLACEMENT_3D('',#14249,#11338,#11339);
#9174=AXIS2_PLACEMENT_3D('',#14251,#11340,#11341);
#9175=AXIS2_PLACEMENT_3D('',#14254,#11343,#11344);
#9176=AXIS2_PLACEMENT_3D('',#14255,#11345,#11346);
#9177=AXIS2_PLACEMENT_3D('',#14256,#11347,#11348);
#9178=AXIS2_PLACEMENT_3D('',#14258,#11349,#11350);
#9179=AXIS2_PLACEMENT_3D('',#14260,#11351,#11352);
#9180=AXIS2_PLACEMENT_3D('',#14261,#11353,#11354);
#9181=AXIS2_PLACEMENT_3D('',#14263,#11355,#11356);
#9182=AXIS2_PLACEMENT_3D('',#14265,#11357,#11358);
#9183=AXIS2_PLACEMENT_3D('',#14266,#11359,#11360);
#9184=AXIS2_PLACEMENT_3D('',#14268,#11362,#11363);
#9185=AXIS2_PLACEMENT_3D('',#14271,#11365,#11366);
#9186=AXIS2_PLACEMENT_3D('',#14272,#11367,#11368);
#9187=AXIS2_PLACEMENT_3D('',#14274,#11369,#11370);
#9188=AXIS2_PLACEMENT_3D('',#14276,#11372,#11373);
#9189=AXIS2_PLACEMENT_3D('',#14277,#11374,#11375);
#9190=AXIS2_PLACEMENT_3D('',#14278,#11376,#11377);
#9191=AXIS2_PLACEMENT_3D('',#14279,#11378,#11379);
#9192=AXIS2_PLACEMENT_3D('',#14281,#11380,#11381);
#9193=AXIS2_PLACEMENT_3D('',#14284,#11383,#11384);
#9194=AXIS2_PLACEMENT_3D('',#14285,#11385,#11386);
#9195=AXIS2_PLACEMENT_3D('',#14287,#11387,#11388);
#9196=AXIS2_PLACEMENT_3D('',#14290,#11390,#11391);
#9197=AXIS2_PLACEMENT_3D('',#14291,#11392,#11393);
#9198=AXIS2_PLACEMENT_3D('',#14292,#11394,#11395);
#9199=AXIS2_PLACEMENT_3D('',#14293,#11396,#11397);
#9200=AXIS2_PLACEMENT_3D('',#14294,#11398,#11399);
#9201=AXIS2_PLACEMENT_3D('',#14296,#11400,#11401);
#9202=AXIS2_PLACEMENT_3D('',#14299,#11403,#11404);
#9203=AXIS2_PLACEMENT_3D('',#14300,#11405,#11406);
#9204=AXIS2_PLACEMENT_3D('',#14302,#11407,#11408);
#9205=AXIS2_PLACEMENT_3D('',#14305,#11410,#11411);
#9206=AXIS2_PLACEMENT_3D('',#14306,#11412,#11413);
#9207=AXIS2_PLACEMENT_3D('',#14307,#11414,#11415);
#9208=AXIS2_PLACEMENT_3D('',#14308,#11416,#11417);
#9209=AXIS2_PLACEMENT_3D('',#14309,#11418,#11419);
#9210=AXIS2_PLACEMENT_3D('',#14311,#11420,#11421);
#9211=AXIS2_PLACEMENT_3D('',#14314,#11423,#11424);
#9212=AXIS2_PLACEMENT_3D('',#14315,#11425,#11426);
#9213=AXIS2_PLACEMENT_3D('',#14317,#11427,#11428);
#9214=AXIS2_PLACEMENT_3D('',#14320,#11430,#11431);
#9215=AXIS2_PLACEMENT_3D('',#14321,#11432,#11433);
#9216=AXIS2_PLACEMENT_3D('',#14322,#11434,#11435);
#9217=AXIS2_PLACEMENT_3D('',#14323,#11436,#11437);
#9218=AXIS2_PLACEMENT_3D('',#14324,#11438,#11439);
#9219=AXIS2_PLACEMENT_3D('',#14325,#11440,#11441);
#9220=AXIS2_PLACEMENT_3D('',#14329,#11443,#11444);
#9221=AXIS2_PLACEMENT_3D('',#14330,#11445,#11446);
#9222=AXIS2_PLACEMENT_3D('',#14334,#11448,#11449);
#9223=AXIS2_PLACEMENT_3D('',#14337,#11451,#11452);
#9224=AXIS2_PLACEMENT_3D('',#14339,#11453,#11454);
#9225=AXIS2_PLACEMENT_3D('',#14341,#11456,#11457);
#9226=AXIS2_PLACEMENT_3D('',#14345,#11459,#11460);
#9227=AXIS2_PLACEMENT_3D('',#14346,#11461,#11462);
#9228=AXIS2_PLACEMENT_3D('',#14350,#11464,#11465);
#9229=AXIS2_PLACEMENT_3D('',#14353,#11467,#11468);
#9230=AXIS2_PLACEMENT_3D('',#14355,#11469,#11470);
#9231=AXIS2_PLACEMENT_3D('',#14357,#11472,#11473);
#9232=AXIS2_PLACEMENT_3D('',#14361,#11475,#11476);
#9233=AXIS2_PLACEMENT_3D('',#14362,#11477,#11478);
#9234=AXIS2_PLACEMENT_3D('',#14366,#11480,#11481);
#9235=AXIS2_PLACEMENT_3D('',#14369,#11483,#11484);
#9236=AXIS2_PLACEMENT_3D('',#14371,#11485,#11486);
#9237=AXIS2_PLACEMENT_3D('',#14373,#11488,#11489);
#9238=AXIS2_PLACEMENT_3D('',#14377,#11491,#11492);
#9239=AXIS2_PLACEMENT_3D('',#14378,#11493,#11494);
#9240=AXIS2_PLACEMENT_3D('',#14382,#11496,#11497);
#9241=AXIS2_PLACEMENT_3D('',#14385,#11499,#11500);
#9242=AXIS2_PLACEMENT_3D('',#14387,#11501,#11502);
#9243=AXIS2_PLACEMENT_3D('',#14389,#11504,#11505);
#9244=AXIS2_PLACEMENT_3D('',#14400,#11512,#11513);
#9245=AXIS2_PLACEMENT_3D('',#14411,#11520,#11521);
#9246=AXIS2_PLACEMENT_3D('',#14430,#11532,#11533);
#9247=AXIS2_PLACEMENT_3D('',#14434,#11536,#11537);
#9248=AXIS2_PLACEMENT_3D('',#14438,#11540,#11541);
#9249=AXIS2_PLACEMENT_3D('',#14442,#11544,#11545);
#9250=AXIS2_PLACEMENT_3D('',#14446,#11548,#11549);
#9251=AXIS2_PLACEMENT_3D('',#14448,#11551,#11552);
#9252=AXIS2_PLACEMENT_3D('',#14452,#11555,#11556);
#9253=AXIS2_PLACEMENT_3D('',#14456,#11559,#11560);
#9254=AXIS2_PLACEMENT_3D('',#14460,#11563,#11564);
#9255=AXIS2_PLACEMENT_3D('',#14464,#11567,#11568);
#9256=AXIS2_PLACEMENT_3D('',#14466,#11570,#11571);
#9257=AXIS2_PLACEMENT_3D('',#14467,#11572,#11573);
#9258=AXIS2_PLACEMENT_3D('',#14468,#11574,#11575);
#9259=AXIS2_PLACEMENT_3D('',#14477,#11580,#11581);
#9260=AXIS2_PLACEMENT_3D('',#14483,#11585,#11586);
#9261=AXIS2_PLACEMENT_3D('',#14489,#11590,#11591);
#9262=AXIS2_PLACEMENT_3D('',#14495,#11595,#11596);
#9263=AXIS2_PLACEMENT_3D('',#14501,#11600,#11601);
#9264=AXIS2_PLACEMENT_3D('',#14507,#11605,#11606);
#9265=AXIS2_PLACEMENT_3D('',#14513,#11610,#11611);
#9266=AXIS2_PLACEMENT_3D('',#14516,#11614,#11615);
#9267=AXIS2_PLACEMENT_3D('',#14517,#11616,#11617);
#9268=AXIS2_PLACEMENT_3D('',#14518,#11618,#11619);
#9269=AXIS2_PLACEMENT_3D('',#14519,#11620,#11621);
#9270=AXIS2_PLACEMENT_3D('',#14528,#11626,#11627);
#9271=AXIS2_PLACEMENT_3D('',#14534,#11631,#11632);
#9272=AXIS2_PLACEMENT_3D('',#14540,#11636,#11637);
#9273=AXIS2_PLACEMENT_3D('',#14546,#11641,#11642);
#9274=AXIS2_PLACEMENT_3D('',#14552,#11646,#11647);
#9275=AXIS2_PLACEMENT_3D('',#14558,#11651,#11652);
#9276=AXIS2_PLACEMENT_3D('',#14564,#11656,#11657);
#9277=AXIS2_PLACEMENT_3D('',#14567,#11660,#11661);
#9278=AXIS2_PLACEMENT_3D('',#14568,#11662,#11663);
#9279=AXIS2_PLACEMENT_3D('',#14569,#11664,#11665);
#9280=AXIS2_PLACEMENT_3D('',#14570,#11666,#11667);
#9281=AXIS2_PLACEMENT_3D('',#14571,#11668,#11669);
#9282=AXIS2_PLACEMENT_3D('',#14572,#11670,#11671);
#9283=AXIS2_PLACEMENT_3D('',#14573,#11672,#11673);
#9284=AXIS2_PLACEMENT_3D('',#14582,#11678,#11679);
#9285=AXIS2_PLACEMENT_3D('',#14588,#11683,#11684);
#9286=AXIS2_PLACEMENT_3D('',#14594,#11688,#11689);
#9287=AXIS2_PLACEMENT_3D('',#14600,#11693,#11694);
#9288=AXIS2_PLACEMENT_3D('',#14606,#11698,#11699);
#9289=AXIS2_PLACEMENT_3D('',#14609,#11702,#11703);
#9290=AXIS2_PLACEMENT_3D('',#14610,#11704,#11705);
#9291=AXIS2_PLACEMENT_3D('',#14611,#11706,#11707);
#9292=AXIS2_PLACEMENT_3D('',#14613,#11708,#11709);
#9293=AXIS2_PLACEMENT_3D('',#14614,#11710,#11711);
#9294=AXIS2_PLACEMENT_3D('',#14616,#11712,#11713);
#9295=AXIS2_PLACEMENT_3D('',#14617,#11714,#11715);
#9296=AXIS2_PLACEMENT_3D('',#14619,#11716,#11717);
#9297=AXIS2_PLACEMENT_3D('',#14621,#11719,#11720);
#9298=AXIS2_PLACEMENT_3D('',#14623,#11721,#11722);
#9299=AXIS2_PLACEMENT_3D('',#14625,#11724,#11725);
#9300=AXIS2_PLACEMENT_3D('',#14627,#11726,#11727);
#9301=AXIS2_PLACEMENT_3D('',#14629,#11729,#11730);
#9302=AXIS2_PLACEMENT_3D('',#14631,#11731,#11732);
#9303=AXIS2_PLACEMENT_3D('',#14632,#11733,#11734);
#9304=AXIS2_PLACEMENT_3D('',#14634,#11735,#11736);
#9305=AXIS2_PLACEMENT_3D('',#14636,#11738,#11739);
#9306=AXIS2_PLACEMENT_3D('',#14638,#11741,#11742);
#9307=AXIS2_PLACEMENT_3D('',#14639,#11743,#11744);
#9308=AXIS2_PLACEMENT_3D('',#14648,#11749,#11750);
#9309=AXIS2_PLACEMENT_3D('',#14654,#11754,#11755);
#9310=AXIS2_PLACEMENT_3D('',#14660,#11759,#11760);
#9311=AXIS2_PLACEMENT_3D('',#14666,#11764,#11765);
#9312=AXIS2_PLACEMENT_3D('',#14672,#11769,#11770);
#9313=AXIS2_PLACEMENT_3D('',#14675,#11773,#11774);
#9314=AXIS2_PLACEMENT_3D('',#14676,#11775,#11776);
#9315=AXIS2_PLACEMENT_3D('',#14677,#11777,#11778);
#9316=AXIS2_PLACEMENT_3D('',#14679,#11779,#11780);
#9317=AXIS2_PLACEMENT_3D('',#14680,#11781,#11782);
#9318=AXIS2_PLACEMENT_3D('',#14682,#11783,#11784);
#9319=AXIS2_PLACEMENT_3D('',#14683,#11785,#11786);
#9320=AXIS2_PLACEMENT_3D('',#14685,#11787,#11788);
#9321=AXIS2_PLACEMENT_3D('',#14687,#11790,#11791);
#9322=AXIS2_PLACEMENT_3D('',#14689,#11792,#11793);
#9323=AXIS2_PLACEMENT_3D('',#14691,#11795,#11796);
#9324=AXIS2_PLACEMENT_3D('',#14693,#11797,#11798);
#9325=AXIS2_PLACEMENT_3D('',#14695,#11800,#11801);
#9326=AXIS2_PLACEMENT_3D('',#14697,#11802,#11803);
#9327=AXIS2_PLACEMENT_3D('',#14698,#11804,#11805);
#9328=AXIS2_PLACEMENT_3D('',#14700,#11806,#11807);
#9329=AXIS2_PLACEMENT_3D('',#14702,#11809,#11810);
#9330=AXIS2_PLACEMENT_3D('',#14704,#11812,#11813);
#9331=AXIS2_PLACEMENT_3D('',#14705,#11814,#11815);
#9332=AXIS2_PLACEMENT_3D('',#14706,#11816,#11817);
#9333=AXIS2_PLACEMENT_3D('',#14707,#11818,#11819);
#9334=AXIS2_PLACEMENT_3D('',#14708,#11820,#11821);
#9335=AXIS2_PLACEMENT_3D('',#14709,#11822,#11823);
#9336=AXIS2_PLACEMENT_3D('',#14710,#11824,#11825);
#9337=AXIS2_PLACEMENT_3D('',#14711,#11826,#11827);
#9338=AXIS2_PLACEMENT_3D('',#14712,#11828,#11829);
#9339=AXIS2_PLACEMENT_3D('',#14713,#11830,#11831);
#9340=AXIS2_PLACEMENT_3D('',#14714,#11832,#11833);
#9341=AXIS2_PLACEMENT_3D('',#14715,#11834,#11835);
#9342=AXIS2_PLACEMENT_3D('',#14716,#11836,#11837);
#9343=AXIS2_PLACEMENT_3D('',#14717,#11838,#11839);
#9344=AXIS2_PLACEMENT_3D('',#14718,#11840,#11841);
#9345=AXIS2_PLACEMENT_3D('',#14719,#11842,#11843);
#9346=AXIS2_PLACEMENT_3D('',#14720,#11844,#11845);
#9347=AXIS2_PLACEMENT_3D('',#14721,#11846,#11847);
#9348=AXIS2_PLACEMENT_3D('',#14722,#11848,#11849);
#9349=AXIS2_PLACEMENT_3D('',#14723,#11850,#11851);
#9350=AXIS2_PLACEMENT_3D('',#14724,#11852,#11853);
#9351=AXIS2_PLACEMENT_3D('',#14725,#11854,#11855);
#9352=AXIS2_PLACEMENT_3D('',#14726,#11856,#11857);
#9353=AXIS2_PLACEMENT_3D('',#14727,#11858,#11859);
#9354=AXIS2_PLACEMENT_3D('',#14728,#11860,#11861);
#9355=AXIS2_PLACEMENT_3D('',#14729,#11862,#11863);
#9356=AXIS2_PLACEMENT_3D('',#14730,#11864,#11865);
#9357=AXIS2_PLACEMENT_3D('',#14731,#11866,#11867);
#9358=AXIS2_PLACEMENT_3D('',#14732,#11868,#11869);
#9359=AXIS2_PLACEMENT_3D('',#14733,#11870,#11871);
#9360=AXIS2_PLACEMENT_3D('',#14734,#11872,#11873);
#9361=AXIS2_PLACEMENT_3D('',#14735,#11874,#11875);
#9362=AXIS2_PLACEMENT_3D('',#14736,#11876,#11877);
#9363=AXIS2_PLACEMENT_3D('',#14737,#11878,#11879);
#9364=AXIS2_PLACEMENT_3D('',#14738,#11880,#11881);
#9365=AXIS2_PLACEMENT_3D('',#14739,#11882,#11883);
#9366=AXIS2_PLACEMENT_3D('',#14740,#11884,#11885);
#9367=AXIS2_PLACEMENT_3D('',#14741,#11886,#11887);
#9368=AXIS2_PLACEMENT_3D('',#14742,#11888,#11889);
#9369=AXIS2_PLACEMENT_3D('',#14743,#11890,#11891);
#9370=AXIS2_PLACEMENT_3D('',#14744,#11892,#11893);
#9371=AXIS2_PLACEMENT_3D('',#14745,#11894,#11895);
#9372=AXIS2_PLACEMENT_3D('',#14746,#11896,#11897);
#9373=AXIS2_PLACEMENT_3D('',#14747,#11898,#11899);
#9374=AXIS2_PLACEMENT_3D('',#14748,#11900,#11901);
#9375=AXIS2_PLACEMENT_3D('',#14749,#11902,#11903);
#9376=AXIS2_PLACEMENT_3D('',#14750,#11904,#11905);
#9377=AXIS2_PLACEMENT_3D('',#14751,#11906,#11907);
#9378=AXIS2_PLACEMENT_3D('',#14752,#11908,#11909);
#9379=AXIS2_PLACEMENT_3D('',#14753,#11910,#11911);
#9380=AXIS2_PLACEMENT_3D('',#14754,#11912,#11913);
#9381=AXIS2_PLACEMENT_3D('',#14755,#11914,#11915);
#9382=AXIS2_PLACEMENT_3D('',#14756,#11916,#11917);
#9383=AXIS2_PLACEMENT_3D('',#14757,#11918,#11919);
#9384=AXIS2_PLACEMENT_3D('',#14758,#11920,#11921);
#9385=AXIS2_PLACEMENT_3D('',#14759,#11922,#11923);
#9386=AXIS2_PLACEMENT_3D('',#14760,#11924,#11925);
#9387=AXIS2_PLACEMENT_3D('',#14761,#11926,#11927);
#9388=AXIS2_PLACEMENT_3D('',#14762,#11928,#11929);
#9389=AXIS2_PLACEMENT_3D('',#14763,#11930,#11931);
#9390=AXIS2_PLACEMENT_3D('',#14764,#11932,#11933);
#9391=AXIS2_PLACEMENT_3D('',#14765,#11934,#11935);
#9392=AXIS2_PLACEMENT_3D('',#14766,#11936,#11937);
#9393=AXIS2_PLACEMENT_3D('',#14767,#11938,#11939);
#9394=AXIS2_PLACEMENT_3D('',#14768,#11940,#11941);
#9395=AXIS2_PLACEMENT_3D('',#14769,#11942,#11943);
#9396=AXIS2_PLACEMENT_3D('',#14770,#11944,#11945);
#9397=DIRECTION('axis',(0.,0.,1.));
#9398=DIRECTION('refdir',(1.,0.,0.));
#9399=DIRECTION('axis',(0.,0.,1.));
#9400=DIRECTION('refdir',(1.,0.,0.));
#9401=DIRECTION('axis',(0.,0.,1.));
#9402=DIRECTION('refdir',(1.,0.,0.));
#9403=DIRECTION('center_axis',(0.,0.,1.));
#9404=DIRECTION('ref_axis',(1.,0.,0.));
#9405=DIRECTION('center_axis',(0.,0.,1.));
#9406=DIRECTION('ref_axis',(1.,0.,0.));
#9407=DIRECTION('',(0.,0.,1.));
#9408=DIRECTION('center_axis',(0.,0.,-1.));
#9409=DIRECTION('ref_axis',(1.,0.,0.));
#9410=DIRECTION('center_axis',(0.,0.,1.));
#9411=DIRECTION('ref_axis',(1.,0.,0.));
#9412=DIRECTION('center_axis',(0.,0.,1.));
#9413=DIRECTION('ref_axis',(1.,0.,0.));
#9414=DIRECTION('',(0.,0.,1.));
#9415=DIRECTION('center_axis',(0.,0.,-1.));
#9416=DIRECTION('ref_axis',(1.,0.,0.));
#9417=DIRECTION('center_axis',(0.,0.,1.));
#9418=DIRECTION('ref_axis',(1.,0.,0.));
#9419=DIRECTION('center_axis',(0.,0.,1.));
#9420=DIRECTION('ref_axis',(1.,0.,0.));
#9421=DIRECTION('',(0.,0.,1.));
#9422=DIRECTION('center_axis',(0.,0.,-1.));
#9423=DIRECTION('ref_axis',(1.,0.,0.));
#9424=DIRECTION('center_axis',(0.,0.,1.));
#9425=DIRECTION('ref_axis',(1.,0.,0.));
#9426=DIRECTION('center_axis',(0.,0.,1.));
#9427=DIRECTION('ref_axis',(1.,0.,0.));
#9428=DIRECTION('',(0.,0.,1.));
#9429=DIRECTION('center_axis',(0.,0.,-1.));
#9430=DIRECTION('ref_axis',(1.,0.,0.));
#9431=DIRECTION('center_axis',(0.,0.,1.));
#9432=DIRECTION('ref_axis',(1.,0.,0.));
#9433=DIRECTION('center_axis',(0.,0.,1.));
#9434=DIRECTION('ref_axis',(1.,0.,0.));
#9435=DIRECTION('',(0.,0.,1.));
#9436=DIRECTION('center_axis',(0.,0.,-1.));
#9437=DIRECTION('ref_axis',(1.,0.,0.));
#9438=DIRECTION('center_axis',(0.,0.,1.));
#9439=DIRECTION('ref_axis',(1.,0.,0.));
#9440=DIRECTION('center_axis',(0.,0.,1.));
#9441=DIRECTION('ref_axis',(1.,0.,0.));
#9442=DIRECTION('',(0.,0.,1.));
#9443=DIRECTION('center_axis',(0.,0.,-1.));
#9444=DIRECTION('ref_axis',(1.,0.,0.));
#9445=DIRECTION('center_axis',(0.,0.,1.));
#9446=DIRECTION('ref_axis',(1.,0.,0.));
#9447=DIRECTION('center_axis',(0.,0.,1.));
#9448=DIRECTION('ref_axis',(1.,0.,0.));
#9449=DIRECTION('',(0.,0.,1.));
#9450=DIRECTION('center_axis',(0.,0.,-1.));
#9451=DIRECTION('ref_axis',(1.,0.,0.));
#9452=DIRECTION('center_axis',(0.,0.,1.));
#9453=DIRECTION('ref_axis',(1.,0.,0.));
#9454=DIRECTION('center_axis',(0.,0.,1.));
#9455=DIRECTION('ref_axis',(1.,0.,0.));
#9456=DIRECTION('',(0.,0.,1.));
#9457=DIRECTION('center_axis',(0.,0.,-1.));
#9458=DIRECTION('ref_axis',(1.,0.,0.));
#9459=DIRECTION('center_axis',(0.,0.,1.));
#9460=DIRECTION('ref_axis',(1.,0.,0.));
#9461=DIRECTION('center_axis',(0.,0.,1.));
#9462=DIRECTION('ref_axis',(1.,0.,0.));
#9463=DIRECTION('',(0.,0.,1.));
#9464=DIRECTION('center_axis',(0.,0.,-1.));
#9465=DIRECTION('ref_axis',(1.,0.,0.));
#9466=DIRECTION('center_axis',(0.,0.,1.));
#9467=DIRECTION('ref_axis',(1.,0.,0.));
#9468=DIRECTION('center_axis',(0.,0.,1.));
#9469=DIRECTION('ref_axis',(1.,0.,0.));
#9470=DIRECTION('',(0.,0.,1.));
#9471=DIRECTION('center_axis',(0.,0.,-1.));
#9472=DIRECTION('ref_axis',(1.,0.,0.));
#9473=DIRECTION('center_axis',(0.,0.,1.));
#9474=DIRECTION('ref_axis',(1.,0.,0.));
#9475=DIRECTION('center_axis',(0.,0.,1.));
#9476=DIRECTION('ref_axis',(1.,0.,0.));
#9477=DIRECTION('',(0.,0.,1.));
#9478=DIRECTION('center_axis',(0.,0.,-1.));
#9479=DIRECTION('ref_axis',(1.,0.,0.));
#9480=DIRECTION('center_axis',(0.,0.,1.));
#9481=DIRECTION('ref_axis',(1.,0.,0.));
#9482=DIRECTION('center_axis',(0.,0.,1.));
#9483=DIRECTION('ref_axis',(1.,0.,0.));
#9484=DIRECTION('',(0.,0.,1.));
#9485=DIRECTION('center_axis',(0.,0.,-1.));
#9486=DIRECTION('ref_axis',(1.,0.,0.));
#9487=DIRECTION('center_axis',(0.,1.,0.));
#9488=DIRECTION('ref_axis',(-1.,0.,0.));
#9489=DIRECTION('',(-1.,0.,0.));
#9490=DIRECTION('',(0.,0.,1.));
#9491=DIRECTION('',(-1.,0.,0.));
#9492=DIRECTION('',(0.,0.,1.));
#9493=DIRECTION('center_axis',(1.,0.,0.));
#9494=DIRECTION('ref_axis',(0.,1.,0.));
#9495=DIRECTION('',(0.,1.,0.));
#9496=DIRECTION('',(0.,1.,0.));
#9497=DIRECTION('',(0.,0.,1.));
#9498=DIRECTION('center_axis',(0.,-1.,0.));
#9499=DIRECTION('ref_axis',(1.,0.,0.));
#9500=DIRECTION('',(1.,0.,0.));
#9501=DIRECTION('',(1.,0.,0.));
#9502=DIRECTION('',(0.,0.,1.));
#9503=DIRECTION('center_axis',(-1.,0.,0.));
#9504=DIRECTION('ref_axis',(0.,-1.,0.));
#9505=DIRECTION('',(0.,-1.,0.));
#9506=DIRECTION('',(0.,-1.,0.));
#9507=DIRECTION('center_axis',(0.,0.,1.));
#9508=DIRECTION('ref_axis',(1.,0.,0.));
#9509=DIRECTION('center_axis',(0.,0.,1.));
#9510=DIRECTION('ref_axis',(1.,0.,0.));
#9511=DIRECTION('axis',(0.,0.,1.));
#9512=DIRECTION('refdir',(1.,0.,0.));
#9513=DIRECTION('center_axis',(0.,1.,0.));
#9514=DIRECTION('ref_axis',(-1.,0.,0.));
#9515=DIRECTION('',(-1.,0.,0.));
#9516=DIRECTION('',(0.,0.,1.));
#9517=DIRECTION('',(-1.,0.,0.));
#9518=DIRECTION('',(0.,0.,1.));
#9519=DIRECTION('center_axis',(1.,0.,0.));
#9520=DIRECTION('ref_axis',(0.,1.,0.));
#9521=DIRECTION('',(0.,1.,0.));
#9522=DIRECTION('',(0.,1.,0.));
#9523=DIRECTION('',(0.,0.,1.));
#9524=DIRECTION('center_axis',(0.,-1.,0.));
#9525=DIRECTION('ref_axis',(1.,0.,0.));
#9526=DIRECTION('',(1.,0.,0.));
#9527=DIRECTION('',(1.,0.,0.));
#9528=DIRECTION('',(0.,0.,1.));
#9529=DIRECTION('center_axis',(-1.,0.,0.));
#9530=DIRECTION('ref_axis',(0.,-1.,0.));
#9531=DIRECTION('',(0.,-1.,0.));
#9532=DIRECTION('',(0.,-1.,0.));
#9533=DIRECTION('center_axis',(0.,0.,1.));
#9534=DIRECTION('ref_axis',(1.,0.,0.));
#9535=DIRECTION('center_axis',(0.,0.,1.));
#9536=DIRECTION('ref_axis',(1.,0.,0.));
#9537=DIRECTION('axis',(0.,0.,1.));
#9538=DIRECTION('refdir',(1.,0.,0.));
#9539=DIRECTION('center_axis',(0.,1.,0.));
#9540=DIRECTION('ref_axis',(-1.,0.,0.));
#9541=DIRECTION('',(-1.,0.,0.));
#9542=DIRECTION('',(0.,0.,1.));
#9543=DIRECTION('',(-1.,0.,0.));
#9544=DIRECTION('',(0.,0.,1.));
#9545=DIRECTION('center_axis',(1.,0.,0.));
#9546=DIRECTION('ref_axis',(0.,1.,0.));
#9547=DIRECTION('',(0.,1.,0.));
#9548=DIRECTION('',(0.,1.,0.));
#9549=DIRECTION('',(0.,0.,1.));
#9550=DIRECTION('center_axis',(0.,-1.,0.));
#9551=DIRECTION('ref_axis',(1.,0.,0.));
#9552=DIRECTION('',(1.,0.,0.));
#9553=DIRECTION('',(1.,0.,0.));
#9554=DIRECTION('',(0.,0.,1.));
#9555=DIRECTION('center_axis',(-1.,0.,0.));
#9556=DIRECTION('ref_axis',(0.,-1.,0.));
#9557=DIRECTION('',(0.,-1.,0.));
#9558=DIRECTION('',(0.,-1.,0.));
#9559=DIRECTION('center_axis',(0.,0.,1.));
#9560=DIRECTION('ref_axis',(1.,0.,0.));
#9561=DIRECTION('center_axis',(0.,0.,1.));
#9562=DIRECTION('ref_axis',(1.,0.,0.));
#9563=DIRECTION('axis',(0.,0.,1.));
#9564=DIRECTION('refdir',(1.,0.,0.));
#9565=DIRECTION('center_axis',(1.,0.,0.));
#9566=DIRECTION('ref_axis',(0.,0.,-1.));
#9567=DIRECTION('',(1.,0.,0.));
#9568=DIRECTION('center_axis',(0.,0.,1.));
#9569=DIRECTION('ref_axis',(1.,0.,0.));
#9570=DIRECTION('center_axis',(0.,0.,1.));
#9571=DIRECTION('ref_axis',(1.,0.,0.));
#9572=DIRECTION('',(0.,0.,1.));
#9573=DIRECTION('center_axis',(0.,0.,-1.));
#9574=DIRECTION('ref_axis',(1.,0.,0.));
#9575=DIRECTION('center_axis',(0.,0.,1.));
#9576=DIRECTION('ref_axis',(1.,0.,0.));
#9577=DIRECTION('center_axis',(0.,0.,1.));
#9578=DIRECTION('ref_axis',(1.,0.,0.));
#9579=DIRECTION('center_axis',(0.,0.,1.));
#9580=DIRECTION('ref_axis',(1.,0.,0.));
#9581=DIRECTION('',(0.,0.,1.));
#9582=DIRECTION('center_axis',(0.,0.,-1.));
#9583=DIRECTION('ref_axis',(1.,0.,0.));
#9584=DIRECTION('center_axis',(0.,0.,1.));
#9585=DIRECTION('ref_axis',(1.,0.,0.));
#9586=DIRECTION('center_axis',(0.,0.,1.));
#9587=DIRECTION('ref_axis',(1.,0.,0.));
#9588=DIRECTION('center_axis',(0.,0.,1.));
#9589=DIRECTION('ref_axis',(1.,0.,0.));
#9590=DIRECTION('',(0.,0.,1.));
#9591=DIRECTION('center_axis',(0.,0.,-1.));
#9592=DIRECTION('ref_axis',(1.,0.,0.));
#9593=DIRECTION('center_axis',(0.,0.,1.));
#9594=DIRECTION('ref_axis',(1.,0.,0.));
#9595=DIRECTION('center_axis',(0.,0.,1.));
#9596=DIRECTION('ref_axis',(1.,0.,0.));
#9597=DIRECTION('center_axis',(0.,0.,1.));
#9598=DIRECTION('ref_axis',(1.,0.,0.));
#9599=DIRECTION('',(0.,0.,1.));
#9600=DIRECTION('center_axis',(0.,0.,-1.));
#9601=DIRECTION('ref_axis',(1.,0.,0.));
#9602=DIRECTION('center_axis',(0.,0.,1.));
#9603=DIRECTION('ref_axis',(1.,0.,0.));
#9604=DIRECTION('center_axis',(0.,0.,1.));
#9605=DIRECTION('ref_axis',(1.,0.,0.));
#9606=DIRECTION('',(0.,0.,-1.));
#9607=DIRECTION('center_axis',(0.,0.,1.));
#9608=DIRECTION('ref_axis',(1.,0.,0.));
#9609=DIRECTION('',(0.,0.,1.));
#9610=DIRECTION('center_axis',(0.,0.,1.));
#9611=DIRECTION('ref_axis',(1.,0.,0.));
#9612=DIRECTION('center_axis',(0.,0.,1.));
#9613=DIRECTION('ref_axis',(1.,0.,0.));
#9614=DIRECTION('center_axis',(0.,0.,1.));
#9615=DIRECTION('ref_axis',(1.,0.,0.));
#9616=DIRECTION('center_axis',(0.,0.,1.));
#9617=DIRECTION('ref_axis',(1.,0.,0.));
#9618=DIRECTION('',(0.,0.,-1.));
#9619=DIRECTION('center_axis',(0.,0.,1.));
#9620=DIRECTION('ref_axis',(1.,0.,0.));
#9621=DIRECTION('',(0.,0.,1.));
#9622=DIRECTION('center_axis',(0.,0.,1.));
#9623=DIRECTION('ref_axis',(1.,0.,0.));
#9624=DIRECTION('center_axis',(0.,0.,1.));
#9625=DIRECTION('ref_axis',(1.,0.,0.));
#9626=DIRECTION('center_axis',(0.,0.,1.));
#9627=DIRECTION('ref_axis',(1.,0.,0.));
#9628=DIRECTION('center_axis',(0.,0.,1.));
#9629=DIRECTION('ref_axis',(-0.707106781186548,-0.707106781186547,0.));
#9630=DIRECTION('',(0.,0.,-1.));
#9631=DIRECTION('center_axis',(0.,0.,1.));
#9632=DIRECTION('ref_axis',(1.,0.,0.));
#9633=DIRECTION('',(0.,0.,1.));
#9634=DIRECTION('center_axis',(0.,0.,1.));
#9635=DIRECTION('ref_axis',(1.,0.,0.));
#9636=DIRECTION('center_axis',(0.,0.,1.));
#9637=DIRECTION('ref_axis',(1.,0.,0.));
#9638=DIRECTION('center_axis',(0.,0.,1.));
#9639=DIRECTION('ref_axis',(1.,0.,0.));
#9640=DIRECTION('center_axis',(0.,0.,1.));
#9641=DIRECTION('ref_axis',(-0.707106781186547,0.707106781186548,0.));
#9642=DIRECTION('',(0.,0.,-1.));
#9643=DIRECTION('center_axis',(0.,0.,1.));
#9644=DIRECTION('ref_axis',(1.,0.,0.));
#9645=DIRECTION('',(0.,0.,1.));
#9646=DIRECTION('center_axis',(0.,0.,1.));
#9647=DIRECTION('ref_axis',(1.,0.,0.));
#9648=DIRECTION('center_axis',(0.,0.,1.));
#9649=DIRECTION('ref_axis',(1.,0.,0.));
#9650=DIRECTION('center_axis',(0.,0.,1.));
#9651=DIRECTION('ref_axis',(1.,0.,0.));
#9652=DIRECTION('center_axis',(0.,0.,1.));
#9653=DIRECTION('ref_axis',(1.,0.,0.));
#9654=DIRECTION('center_axis',(0.,0.,1.));
#9655=DIRECTION('ref_axis',(1.,0.,0.));
#9656=DIRECTION('center_axis',(0.,0.,1.));
#9657=DIRECTION('ref_axis',(1.,0.,0.));
#9658=DIRECTION('center_axis',(0.,0.,1.));
#9659=DIRECTION('ref_axis',(1.,0.,0.));
#9660=DIRECTION('center_axis',(0.,0.,1.));
#9661=DIRECTION('ref_axis',(1.,0.,0.));
#9662=DIRECTION('center_axis',(0.,0.,1.));
#9663=DIRECTION('ref_axis',(1.,0.,0.));
#9664=DIRECTION('center_axis',(0.,0.,1.));
#9665=DIRECTION('ref_axis',(1.,0.,0.));
#9666=DIRECTION('center_axis',(0.,0.,-1.));
#9667=DIRECTION('ref_axis',(1.,0.,0.));
#9668=DIRECTION('center_axis',(0.,0.,-1.));
#9669=DIRECTION('ref_axis',(1.,0.,0.));
#9670=DIRECTION('center_axis',(0.,0.,-1.));
#9671=DIRECTION('ref_axis',(1.,0.,0.));
#9672=DIRECTION('center_axis',(0.,0.,-1.));
#9673=DIRECTION('ref_axis',(1.,0.,0.));
#9674=DIRECTION('center_axis',(0.,0.,1.));
#9675=DIRECTION('ref_axis',(1.,0.,0.));
#9676=DIRECTION('center_axis',(0.,0.,1.));
#9677=DIRECTION('ref_axis',(1.,0.,0.));
#9678=DIRECTION('',(0.,0.,1.));
#9679=DIRECTION('center_axis',(0.,0.,1.));
#9680=DIRECTION('ref_axis',(1.,0.,0.));
#9681=DIRECTION('center_axis',(0.,0.,1.));
#9682=DIRECTION('ref_axis',(1.,0.,0.));
#9683=DIRECTION('',(0.,0.,1.));
#9684=DIRECTION('center_axis',(0.,0.,1.));
#9685=DIRECTION('ref_axis',(1.,0.,0.));
#9686=DIRECTION('center_axis',(0.,0.,1.));
#9687=DIRECTION('ref_axis',(1.,0.,0.));
#9688=DIRECTION('',(0.,0.,1.));
#9689=DIRECTION('center_axis',(0.,0.,1.));
#9690=DIRECTION('ref_axis',(1.,0.,0.));
#9691=DIRECTION('center_axis',(0.,0.,1.));
#9692=DIRECTION('ref_axis',(1.,0.,0.));
#9693=DIRECTION('',(0.,0.,1.));
#9694=DIRECTION('center_axis',(0.,0.,1.));
#9695=DIRECTION('ref_axis',(1.,0.,0.));
#9696=DIRECTION('center_axis',(0.,0.,1.));
#9697=DIRECTION('ref_axis',(1.,0.,0.));
#9698=DIRECTION('',(0.,0.,-1.));
#9699=DIRECTION('center_axis',(0.,0.,1.));
#9700=DIRECTION('ref_axis',(1.,0.,0.));
#9701=DIRECTION('center_axis',(0.,0.,1.));
#9702=DIRECTION('ref_axis',(1.,0.,0.));
#9703=DIRECTION('',(0.,0.,1.));
#9704=DIRECTION('center_axis',(0.,0.,-1.));
#9705=DIRECTION('ref_axis',(1.,0.,0.));
#9706=DIRECTION('center_axis',(0.,0.,1.));
#9707=DIRECTION('ref_axis',(1.,0.,0.));
#9708=DIRECTION('center_axis',(0.,0.,1.));
#9709=DIRECTION('ref_axis',(1.,0.,0.));
#9710=DIRECTION('center_axis',(0.,0.,1.));
#9711=DIRECTION('ref_axis',(1.,0.,0.));
#9712=DIRECTION('',(0.,0.,-1.));
#9713=DIRECTION('center_axis',(0.,0.,1.));
#9714=DIRECTION('ref_axis',(1.,0.,0.));
#9715=DIRECTION('center_axis',(0.,0.,1.));
#9716=DIRECTION('ref_axis',(1.,0.,0.));
#9717=DIRECTION('',(0.,0.,-1.));
#9718=DIRECTION('center_axis',(0.,0.,-1.));
#9719=DIRECTION('ref_axis',(1.,0.,0.));
#9720=DIRECTION('center_axis',(0.,0.,1.));
#9721=DIRECTION('ref_axis',(1.,0.,0.));
#9722=DIRECTION('center_axis',(0.,0.,1.));
#9723=DIRECTION('ref_axis',(1.,0.,0.));
#9724=DIRECTION('axis',(0.,0.,1.));
#9725=DIRECTION('refdir',(1.,0.,0.));
#9726=DIRECTION('center_axis',(0.,0.,1.));
#9727=DIRECTION('ref_axis',(1.,0.,0.));
#9728=DIRECTION('center_axis',(0.,0.,1.));
#9729=DIRECTION('ref_axis',(1.,0.,0.));
#9730=DIRECTION('',(0.,0.,1.));
#9731=DIRECTION('center_axis',(0.,0.,-1.));
#9732=DIRECTION('ref_axis',(1.,0.,0.));
#9733=DIRECTION('center_axis',(0.,0.,1.));
#9734=DIRECTION('ref_axis',(1.,0.,0.));
#9735=DIRECTION('center_axis',(0.,0.,1.));
#9736=DIRECTION('ref_axis',(1.,0.,0.));
#9737=DIRECTION('center_axis',(0.,0.,1.));
#9738=DIRECTION('ref_axis',(1.,0.,0.));
#9739=DIRECTION('center_axis',(0.,0.,1.));
#9740=DIRECTION('ref_axis',(1.,0.,0.));
#9741=DIRECTION('',(0.,0.,1.));
#9742=DIRECTION('center_axis',(0.,0.,-1.));
#9743=DIRECTION('ref_axis',(1.,0.,0.));
#9744=DIRECTION('center_axis',(0.,0.,1.));
#9745=DIRECTION('ref_axis',(1.,0.,0.));
#9746=DIRECTION('center_axis',(0.,0.,1.));
#9747=DIRECTION('ref_axis',(1.,0.,0.));
#9748=DIRECTION('center_axis',(0.,0.,1.));
#9749=DIRECTION('ref_axis',(1.,0.,0.));
#9750=DIRECTION('center_axis',(0.,0.,1.));
#9751=DIRECTION('ref_axis',(1.,0.,0.));
#9752=DIRECTION('',(0.,0.,1.));
#9753=DIRECTION('center_axis',(0.,0.,-1.));
#9754=DIRECTION('ref_axis',(1.,0.,0.));
#9755=DIRECTION('center_axis',(0.,0.,1.));
#9756=DIRECTION('ref_axis',(1.,0.,0.));
#9757=DIRECTION('center_axis',(0.,0.,1.));
#9758=DIRECTION('ref_axis',(1.,0.,0.));
#9759=DIRECTION('center_axis',(0.,0.,1.));
#9760=DIRECTION('ref_axis',(1.,0.,0.));
#9761=DIRECTION('center_axis',(0.,0.,1.));
#9762=DIRECTION('ref_axis',(1.,0.,0.));
#9763=DIRECTION('',(0.,0.,1.));
#9764=DIRECTION('center_axis',(0.,0.,-1.));
#9765=DIRECTION('ref_axis',(1.,0.,0.));
#9766=DIRECTION('center_axis',(0.,0.,1.));
#9767=DIRECTION('ref_axis',(1.,0.,0.));
#9768=DIRECTION('center_axis',(0.,0.,1.));
#9769=DIRECTION('ref_axis',(1.,0.,0.));
#9770=DIRECTION('center_axis',(0.,0.,1.));
#9771=DIRECTION('ref_axis',(1.,0.,0.));
#9772=DIRECTION('center_axis',(0.,0.,1.));
#9773=DIRECTION('ref_axis',(1.,0.,0.));
#9774=DIRECTION('',(0.,0.,1.));
#9775=DIRECTION('center_axis',(0.,0.,1.));
#9776=DIRECTION('ref_axis',(1.,0.,0.));
#9777=DIRECTION('center_axis',(0.,0.,1.));
#9778=DIRECTION('ref_axis',(1.,0.,0.));
#9779=DIRECTION('',(0.,0.,1.));
#9780=DIRECTION('center_axis',(0.,0.,1.));
#9781=DIRECTION('ref_axis',(1.,0.,0.));
#9782=DIRECTION('center_axis',(0.,0.,1.));
#9783=DIRECTION('ref_axis',(1.,0.,0.));
#9784=DIRECTION('',(0.,0.,1.));
#9785=DIRECTION('center_axis',(0.,0.,1.));
#9786=DIRECTION('ref_axis',(1.,0.,0.));
#9787=DIRECTION('center_axis',(0.,0.,1.));
#9788=DIRECTION('ref_axis',(1.,0.,0.));
#9789=DIRECTION('',(0.,0.,1.));
#9790=DIRECTION('center_axis',(0.,0.,1.));
#9791=DIRECTION('ref_axis',(1.,0.,0.));
#9792=DIRECTION('center_axis',(0.,0.,1.));
#9793=DIRECTION('ref_axis',(1.,0.,0.));
#9794=DIRECTION('',(0.,0.,-1.));
#9795=DIRECTION('center_axis',(0.,0.,1.));
#9796=DIRECTION('ref_axis',(1.,0.,0.));
#9797=DIRECTION('center_axis',(0.,0.,1.));
#9798=DIRECTION('ref_axis',(1.,0.,0.));
#9799=DIRECTION('center_axis',(0.,0.,-1.));
#9800=DIRECTION('ref_axis',(1.,0.,0.));
#9801=DIRECTION('center_axis',(0.,0.,1.));
#9802=DIRECTION('ref_axis',(1.,0.,0.));
#9803=DIRECTION('center_axis',(0.,0.,-1.));
#9804=DIRECTION('ref_axis',(1.,0.,0.));
#9805=DIRECTION('',(0.,0.,-1.));
#9806=DIRECTION('center_axis',(0.,0.,1.));
#9807=DIRECTION('ref_axis',(1.,0.,0.));
#9808=DIRECTION('center_axis',(0.,0.,1.));
#9809=DIRECTION('ref_axis',(1.,0.,0.));
#9810=DIRECTION('',(0.,0.,-1.));
#9811=DIRECTION('center_axis',(0.,0.,1.));
#9812=DIRECTION('ref_axis',(1.,0.,0.));
#9813=DIRECTION('center_axis',(0.,0.,1.));
#9814=DIRECTION('ref_axis',(1.,0.,0.));
#9815=DIRECTION('center_axis',(0.,0.,1.));
#9816=DIRECTION('ref_axis',(1.,0.,0.));
#9817=DIRECTION('axis',(0.,0.,1.));
#9818=DIRECTION('refdir',(1.,0.,0.));
#9819=DIRECTION('center_axis',(1.,0.,0.));
#9820=DIRECTION('ref_axis',(0.,0.,-1.));
#9821=DIRECTION('',(1.,0.,0.));
#9822=DIRECTION('center_axis',(0.,0.,1.));
#9823=DIRECTION('ref_axis',(1.,0.,0.));
#9824=DIRECTION('center_axis',(0.,0.,1.));
#9825=DIRECTION('ref_axis',(1.,0.,0.));
#9826=DIRECTION('',(0.,0.,1.));
#9827=DIRECTION('center_axis',(0.,0.,-1.));
#9828=DIRECTION('ref_axis',(1.,0.,0.));
#9829=DIRECTION('center_axis',(0.,0.,1.));
#9830=DIRECTION('ref_axis',(1.,0.,0.));
#9831=DIRECTION('center_axis',(0.,0.,1.));
#9832=DIRECTION('ref_axis',(1.,0.,0.));
#9833=DIRECTION('center_axis',(0.,0.,1.));
#9834=DIRECTION('ref_axis',(1.,0.,0.));
#9835=DIRECTION('',(0.,0.,1.));
#9836=DIRECTION('center_axis',(0.,0.,-1.));
#9837=DIRECTION('ref_axis',(1.,0.,0.));
#9838=DIRECTION('center_axis',(0.,0.,1.));
#9839=DIRECTION('ref_axis',(1.,0.,0.));
#9840=DIRECTION('center_axis',(0.,0.,1.));
#9841=DIRECTION('ref_axis',(1.,0.,0.));
#9842=DIRECTION('center_axis',(0.,0.,1.));
#9843=DIRECTION('ref_axis',(1.,0.,0.));
#9844=DIRECTION('',(0.,0.,1.));
#9845=DIRECTION('center_axis',(0.,0.,-1.));
#9846=DIRECTION('ref_axis',(1.,0.,0.));
#9847=DIRECTION('center_axis',(0.,0.,1.));
#9848=DIRECTION('ref_axis',(1.,0.,0.));
#9849=DIRECTION('center_axis',(0.,0.,1.));
#9850=DIRECTION('ref_axis',(1.,0.,0.));
#9851=DIRECTION('center_axis',(0.,0.,1.));
#9852=DIRECTION('ref_axis',(1.,0.,0.));
#9853=DIRECTION('',(0.,0.,1.));
#9854=DIRECTION('center_axis',(0.,0.,-1.));
#9855=DIRECTION('ref_axis',(1.,0.,0.));
#9856=DIRECTION('center_axis',(0.,0.,1.));
#9857=DIRECTION('ref_axis',(1.,0.,0.));
#9858=DIRECTION('center_axis',(0.,0.,1.));
#9859=DIRECTION('ref_axis',(1.,0.,0.));
#9860=DIRECTION('',(0.,0.,-1.));
#9861=DIRECTION('center_axis',(0.,0.,1.));
#9862=DIRECTION('ref_axis',(1.,0.,0.));
#9863=DIRECTION('',(0.,0.,1.));
#9864=DIRECTION('center_axis',(0.,0.,1.));
#9865=DIRECTION('ref_axis',(1.,0.,0.));
#9866=DIRECTION('center_axis',(0.,0.,1.));
#9867=DIRECTION('ref_axis',(1.,0.,0.));
#9868=DIRECTION('center_axis',(0.,0.,1.));
#9869=DIRECTION('ref_axis',(1.,0.,0.));
#9870=DIRECTION('center_axis',(0.,0.,1.));
#9871=DIRECTION('ref_axis',(1.,0.,0.));
#9872=DIRECTION('',(0.,0.,-1.));
#9873=DIRECTION('center_axis',(0.,0.,1.));
#9874=DIRECTION('ref_axis',(1.,0.,0.));
#9875=DIRECTION('',(0.,0.,1.));
#9876=DIRECTION('center_axis',(0.,0.,1.));
#9877=DIRECTION('ref_axis',(1.,0.,0.));
#9878=DIRECTION('center_axis',(0.,0.,1.));
#9879=DIRECTION('ref_axis',(1.,0.,0.));
#9880=DIRECTION('center_axis',(0.,0.,1.));
#9881=DIRECTION('ref_axis',(1.,0.,0.));
#9882=DIRECTION('center_axis',(0.,0.,1.));
#9883=DIRECTION('ref_axis',(-0.707106781186548,-0.707106781186547,0.));
#9884=DIRECTION('',(0.,0.,-1.));
#9885=DIRECTION('center_axis',(0.,0.,1.));
#9886=DIRECTION('ref_axis',(1.,0.,0.));
#9887=DIRECTION('',(0.,0.,1.));
#9888=DIRECTION('center_axis',(0.,0.,1.));
#9889=DIRECTION('ref_axis',(1.,0.,0.));
#9890=DIRECTION('center_axis',(0.,0.,1.));
#9891=DIRECTION('ref_axis',(1.,0.,0.));
#9892=DIRECTION('center_axis',(0.,0.,1.));
#9893=DIRECTION('ref_axis',(1.,0.,0.));
#9894=DIRECTION('center_axis',(0.,0.,1.));
#9895=DIRECTION('ref_axis',(-0.707106781186547,0.707106781186548,0.));
#9896=DIRECTION('',(0.,0.,-1.));
#9897=DIRECTION('center_axis',(0.,0.,1.));
#9898=DIRECTION('ref_axis',(1.,0.,0.));
#9899=DIRECTION('',(0.,0.,1.));
#9900=DIRECTION('center_axis',(0.,0.,1.));
#9901=DIRECTION('ref_axis',(1.,0.,0.));
#9902=DIRECTION('center_axis',(0.,0.,1.));
#9903=DIRECTION('ref_axis',(1.,0.,0.));
#9904=DIRECTION('center_axis',(0.,0.,1.));
#9905=DIRECTION('ref_axis',(1.,0.,0.));
#9906=DIRECTION('center_axis',(0.,0.,1.));
#9907=DIRECTION('ref_axis',(1.,0.,0.));
#9908=DIRECTION('center_axis',(0.,0.,1.));
#9909=DIRECTION('ref_axis',(1.,0.,0.));
#9910=DIRECTION('center_axis',(0.,0.,1.));
#9911=DIRECTION('ref_axis',(1.,0.,0.));
#9912=DIRECTION('center_axis',(0.,0.,1.));
#9913=DIRECTION('ref_axis',(1.,0.,0.));
#9914=DIRECTION('center_axis',(0.,0.,1.));
#9915=DIRECTION('ref_axis',(1.,0.,0.));
#9916=DIRECTION('center_axis',(0.,0.,1.));
#9917=DIRECTION('ref_axis',(1.,0.,0.));
#9918=DIRECTION('center_axis',(0.,0.,1.));
#9919=DIRECTION('ref_axis',(1.,0.,0.));
#9920=DIRECTION('center_axis',(0.,0.,-1.));
#9921=DIRECTION('ref_axis',(1.,0.,0.));
#9922=DIRECTION('center_axis',(0.,0.,-1.));
#9923=DIRECTION('ref_axis',(1.,0.,0.));
#9924=DIRECTION('center_axis',(0.,0.,-1.));
#9925=DIRECTION('ref_axis',(1.,0.,0.));
#9926=DIRECTION('center_axis',(0.,0.,-1.));
#9927=DIRECTION('ref_axis',(1.,0.,0.));
#9928=DIRECTION('center_axis',(0.,0.,1.));
#9929=DIRECTION('ref_axis',(1.,0.,0.));
#9930=DIRECTION('center_axis',(0.,0.,1.));
#9931=DIRECTION('ref_axis',(1.,0.,0.));
#9932=DIRECTION('',(0.,0.,1.));
#9933=DIRECTION('center_axis',(0.,0.,1.));
#9934=DIRECTION('ref_axis',(1.,0.,0.));
#9935=DIRECTION('center_axis',(0.,0.,1.));
#9936=DIRECTION('ref_axis',(1.,0.,0.));
#9937=DIRECTION('',(0.,0.,1.));
#9938=DIRECTION('center_axis',(0.,0.,1.));
#9939=DIRECTION('ref_axis',(1.,0.,0.));
#9940=DIRECTION('center_axis',(0.,0.,1.));
#9941=DIRECTION('ref_axis',(1.,0.,0.));
#9942=DIRECTION('',(0.,0.,1.));
#9943=DIRECTION('center_axis',(0.,0.,1.));
#9944=DIRECTION('ref_axis',(1.,0.,0.));
#9945=DIRECTION('center_axis',(0.,0.,1.));
#9946=DIRECTION('ref_axis',(1.,0.,0.));
#9947=DIRECTION('',(0.,0.,1.));
#9948=DIRECTION('center_axis',(0.,0.,1.));
#9949=DIRECTION('ref_axis',(1.,0.,0.));
#9950=DIRECTION('center_axis',(0.,0.,1.));
#9951=DIRECTION('ref_axis',(1.,0.,0.));
#9952=DIRECTION('',(0.,0.,-1.));
#9953=DIRECTION('center_axis',(0.,0.,1.));
#9954=DIRECTION('ref_axis',(1.,0.,0.));
#9955=DIRECTION('center_axis',(0.,0.,1.));
#9956=DIRECTION('ref_axis',(1.,0.,0.));
#9957=DIRECTION('',(0.,0.,1.));
#9958=DIRECTION('center_axis',(0.,0.,-1.));
#9959=DIRECTION('ref_axis',(1.,0.,0.));
#9960=DIRECTION('center_axis',(0.,0.,1.));
#9961=DIRECTION('ref_axis',(1.,0.,0.));
#9962=DIRECTION('center_axis',(0.,0.,1.));
#9963=DIRECTION('ref_axis',(1.,0.,0.));
#9964=DIRECTION('center_axis',(0.,0.,1.));
#9965=DIRECTION('ref_axis',(1.,0.,0.));
#9966=DIRECTION('',(0.,0.,-1.));
#9967=DIRECTION('center_axis',(0.,0.,1.));
#9968=DIRECTION('ref_axis',(1.,0.,0.));
#9969=DIRECTION('center_axis',(0.,0.,1.));
#9970=DIRECTION('ref_axis',(1.,0.,0.));
#9971=DIRECTION('',(0.,0.,-1.));
#9972=DIRECTION('center_axis',(0.,0.,-1.));
#9973=DIRECTION('ref_axis',(1.,0.,0.));
#9974=DIRECTION('center_axis',(0.,0.,1.));
#9975=DIRECTION('ref_axis',(1.,0.,0.));
#9976=DIRECTION('center_axis',(0.,0.,1.));
#9977=DIRECTION('ref_axis',(1.,0.,0.));
#9978=DIRECTION('axis',(0.,0.,1.));
#9979=DIRECTION('refdir',(1.,0.,0.));
#9980=DIRECTION('center_axis',(0.,0.,1.));
#9981=DIRECTION('ref_axis',(1.,0.,0.));
#9982=DIRECTION('center_axis',(0.,0.,1.));
#9983=DIRECTION('ref_axis',(1.,0.,0.));
#9984=DIRECTION('',(0.,0.,1.));
#9985=DIRECTION('center_axis',(0.,0.,-1.));
#9986=DIRECTION('ref_axis',(1.,0.,0.));
#9987=DIRECTION('center_axis',(0.,0.,1.));
#9988=DIRECTION('ref_axis',(1.,0.,0.));
#9989=DIRECTION('center_axis',(0.,0.,1.));
#9990=DIRECTION('ref_axis',(1.,0.,0.));
#9991=DIRECTION('center_axis',(0.,0.,1.));
#9992=DIRECTION('ref_axis',(1.,0.,0.));
#9993=DIRECTION('center_axis',(0.,0.,1.));
#9994=DIRECTION('ref_axis',(1.,0.,0.));
#9995=DIRECTION('',(0.,0.,1.));
#9996=DIRECTION('center_axis',(0.,0.,-1.));
#9997=DIRECTION('ref_axis',(1.,0.,0.));
#9998=DIRECTION('center_axis',(0.,0.,1.));
#9999=DIRECTION('ref_axis',(1.,0.,0.));
#10000=DIRECTION('center_axis',(0.,0.,1.));
#10001=DIRECTION('ref_axis',(1.,0.,0.));
#10002=DIRECTION('center_axis',(0.,0.,1.));
#10003=DIRECTION('ref_axis',(1.,0.,0.));
#10004=DIRECTION('center_axis',(0.,0.,1.));
#10005=DIRECTION('ref_axis',(1.,0.,0.));
#10006=DIRECTION('',(0.,0.,1.));
#10007=DIRECTION('center_axis',(0.,0.,-1.));
#10008=DIRECTION('ref_axis',(1.,0.,0.));
#10009=DIRECTION('center_axis',(0.,0.,1.));
#10010=DIRECTION('ref_axis',(1.,0.,0.));
#10011=DIRECTION('center_axis',(0.,0.,1.));
#10012=DIRECTION('ref_axis',(1.,0.,0.));
#10013=DIRECTION('center_axis',(0.,0.,1.));
#10014=DIRECTION('ref_axis',(1.,0.,0.));
#10015=DIRECTION('center_axis',(0.,0.,1.));
#10016=DIRECTION('ref_axis',(1.,0.,0.));
#10017=DIRECTION('',(0.,0.,1.));
#10018=DIRECTION('center_axis',(0.,0.,-1.));
#10019=DIRECTION('ref_axis',(1.,0.,0.));
#10020=DIRECTION('center_axis',(0.,0.,1.));
#10021=DIRECTION('ref_axis',(1.,0.,0.));
#10022=DIRECTION('center_axis',(0.,0.,1.));
#10023=DIRECTION('ref_axis',(1.,0.,0.));
#10024=DIRECTION('center_axis',(0.,0.,1.));
#10025=DIRECTION('ref_axis',(1.,0.,0.));
#10026=DIRECTION('center_axis',(0.,0.,1.));
#10027=DIRECTION('ref_axis',(1.,0.,0.));
#10028=DIRECTION('',(0.,0.,1.));
#10029=DIRECTION('center_axis',(0.,0.,1.));
#10030=DIRECTION('ref_axis',(1.,0.,0.));
#10031=DIRECTION('center_axis',(0.,0.,1.));
#10032=DIRECTION('ref_axis',(1.,0.,0.));
#10033=DIRECTION('',(0.,0.,1.));
#10034=DIRECTION('center_axis',(0.,0.,1.));
#10035=DIRECTION('ref_axis',(1.,0.,0.));
#10036=DIRECTION('center_axis',(0.,0.,1.));
#10037=DIRECTION('ref_axis',(1.,0.,0.));
#10038=DIRECTION('',(0.,0.,1.));
#10039=DIRECTION('center_axis',(0.,0.,1.));
#10040=DIRECTION('ref_axis',(1.,0.,0.));
#10041=DIRECTION('center_axis',(0.,0.,1.));
#10042=DIRECTION('ref_axis',(1.,0.,0.));
#10043=DIRECTION('',(0.,0.,1.));
#10044=DIRECTION('center_axis',(0.,0.,1.));
#10045=DIRECTION('ref_axis',(1.,0.,0.));
#10046=DIRECTION('center_axis',(0.,0.,1.));
#10047=DIRECTION('ref_axis',(1.,0.,0.));
#10048=DIRECTION('',(0.,0.,-1.));
#10049=DIRECTION('center_axis',(0.,0.,1.));
#10050=DIRECTION('ref_axis',(1.,0.,0.));
#10051=DIRECTION('center_axis',(0.,0.,1.));
#10052=DIRECTION('ref_axis',(1.,0.,0.));
#10053=DIRECTION('center_axis',(0.,0.,-1.));
#10054=DIRECTION('ref_axis',(1.,0.,0.));
#10055=DIRECTION('center_axis',(0.,0.,1.));
#10056=DIRECTION('ref_axis',(1.,0.,0.));
#10057=DIRECTION('center_axis',(0.,0.,-1.));
#10058=DIRECTION('ref_axis',(1.,0.,0.));
#10059=DIRECTION('',(0.,0.,-1.));
#10060=DIRECTION('center_axis',(0.,0.,1.));
#10061=DIRECTION('ref_axis',(1.,0.,0.));
#10062=DIRECTION('center_axis',(0.,0.,1.));
#10063=DIRECTION('ref_axis',(1.,0.,0.));
#10064=DIRECTION('',(0.,0.,-1.));
#10065=DIRECTION('center_axis',(0.,0.,1.));
#10066=DIRECTION('ref_axis',(1.,0.,0.));
#10067=DIRECTION('center_axis',(0.,0.,1.));
#10068=DIRECTION('ref_axis',(1.,0.,0.));
#10069=DIRECTION('center_axis',(0.,0.,1.));
#10070=DIRECTION('ref_axis',(1.,0.,0.));
#10071=DIRECTION('axis',(0.,0.,1.));
#10072=DIRECTION('refdir',(1.,0.,0.));
#10073=DIRECTION('center_axis',(0.,0.,1.));
#10074=DIRECTION('ref_axis',(1.,0.,0.));
#10075=DIRECTION('center_axis',(0.,0.,1.));
#10076=DIRECTION('ref_axis',(1.,0.,0.));
#10077=DIRECTION('',(0.,0.,1.));
#10078=DIRECTION('center_axis',(0.,0.,-1.));
#10079=DIRECTION('ref_axis',(1.,0.,0.));
#10080=DIRECTION('center_axis',(0.,0.,1.));
#10081=DIRECTION('ref_axis',(1.,0.,0.));
#10082=DIRECTION('center_axis',(0.,0.,1.));
#10083=DIRECTION('ref_axis',(1.,0.,0.));
#10084=DIRECTION('center_axis',(0.,0.,1.));
#10085=DIRECTION('ref_axis',(1.,0.,0.));
#10086=DIRECTION('center_axis',(0.,0.,1.));
#10087=DIRECTION('ref_axis',(1.,0.,0.));
#10088=DIRECTION('',(0.,0.,1.));
#10089=DIRECTION('center_axis',(0.,0.,-1.));
#10090=DIRECTION('ref_axis',(1.,0.,0.));
#10091=DIRECTION('center_axis',(0.,0.,1.));
#10092=DIRECTION('ref_axis',(1.,0.,0.));
#10093=DIRECTION('center_axis',(0.,0.,1.));
#10094=DIRECTION('ref_axis',(1.,0.,0.));
#10095=DIRECTION('center_axis',(0.,0.,1.));
#10096=DIRECTION('ref_axis',(1.,0.,0.));
#10097=DIRECTION('center_axis',(0.,0.,1.));
#10098=DIRECTION('ref_axis',(1.,0.,0.));
#10099=DIRECTION('',(0.,0.,1.));
#10100=DIRECTION('center_axis',(0.,0.,-1.));
#10101=DIRECTION('ref_axis',(1.,0.,0.));
#10102=DIRECTION('center_axis',(0.,0.,1.));
#10103=DIRECTION('ref_axis',(1.,0.,0.));
#10104=DIRECTION('center_axis',(0.,0.,1.));
#10105=DIRECTION('ref_axis',(1.,0.,0.));
#10106=DIRECTION('center_axis',(0.,0.,1.));
#10107=DIRECTION('ref_axis',(1.,0.,0.));
#10108=DIRECTION('center_axis',(0.,0.,1.));
#10109=DIRECTION('ref_axis',(1.,0.,0.));
#10110=DIRECTION('',(0.,0.,1.));
#10111=DIRECTION('center_axis',(0.,0.,-1.));
#10112=DIRECTION('ref_axis',(1.,0.,0.));
#10113=DIRECTION('center_axis',(0.,0.,1.));
#10114=DIRECTION('ref_axis',(1.,0.,0.));
#10115=DIRECTION('center_axis',(0.,0.,1.));
#10116=DIRECTION('ref_axis',(1.,0.,0.));
#10117=DIRECTION('center_axis',(0.,0.,1.));
#10118=DIRECTION('ref_axis',(1.,0.,0.));
#10119=DIRECTION('center_axis',(0.,0.,1.));
#10120=DIRECTION('ref_axis',(1.,0.,0.));
#10121=DIRECTION('',(0.,0.,1.));
#10122=DIRECTION('center_axis',(0.,0.,1.));
#10123=DIRECTION('ref_axis',(1.,0.,0.));
#10124=DIRECTION('center_axis',(0.,0.,1.));
#10125=DIRECTION('ref_axis',(1.,0.,0.));
#10126=DIRECTION('',(0.,0.,1.));
#10127=DIRECTION('center_axis',(0.,0.,1.));
#10128=DIRECTION('ref_axis',(1.,0.,0.));
#10129=DIRECTION('center_axis',(0.,0.,1.));
#10130=DIRECTION('ref_axis',(1.,0.,0.));
#10131=DIRECTION('',(0.,0.,1.));
#10132=DIRECTION('center_axis',(0.,0.,1.));
#10133=DIRECTION('ref_axis',(1.,0.,0.));
#10134=DIRECTION('center_axis',(0.,0.,1.));
#10135=DIRECTION('ref_axis',(1.,0.,0.));
#10136=DIRECTION('',(0.,0.,1.));
#10137=DIRECTION('center_axis',(0.,-0.56333682464151,0.826227342807548));
#10138=DIRECTION('ref_axis',(0.,-0.826227342807548,-0.56333682464151));
#10139=DIRECTION('',(0.,-0.826227342807548,-0.56333682464151));
#10140=DIRECTION('',(1.,0.,0.));
#10141=DIRECTION('',(0.,-0.826227342807548,-0.56333682464151));
#10142=DIRECTION('',(1.,0.,0.));
#10143=DIRECTION('center_axis',(0.,-1.,0.));
#10144=DIRECTION('ref_axis',(0.,0.,-1.));
#10145=DIRECTION('',(0.,0.,-1.));
#10146=DIRECTION('',(0.,0.,-1.));
#10147=DIRECTION('',(1.,0.,0.));
#10148=DIRECTION('center_axis',(0.,-0.56333682464151,-0.826227342807548));
#10149=DIRECTION('ref_axis',(0.,0.826227342807548,-0.56333682464151));
#10150=DIRECTION('',(0.,0.826227342807548,-0.56333682464151));
#10151=DIRECTION('',(0.,0.826227342807548,-0.56333682464151));
#10152=DIRECTION('',(1.,0.,0.));
#10153=DIRECTION('center_axis',(0.,-1.,0.));
#10154=DIRECTION('ref_axis',(0.,0.,-1.));
#10155=DIRECTION('',(0.,0.,-1.));
#10156=DIRECTION('',(0.,0.,-1.));
#10157=DIRECTION('',(1.,0.,0.));
#10158=DIRECTION('center_axis',(0.,0.,1.));
#10159=DIRECTION('ref_axis',(0.,-1.,0.));
#10160=DIRECTION('',(0.,-1.,0.));
#10161=DIRECTION('',(0.,-1.,0.));
#10162=DIRECTION('',(1.,0.,0.));
#10163=DIRECTION('center_axis',(0.,1.,0.));
#10164=DIRECTION('ref_axis',(0.,0.,1.));
#10165=DIRECTION('',(0.,0.,1.));
#10166=DIRECTION('',(0.,0.,1.));
#10167=DIRECTION('',(1.,0.,0.));
#10168=DIRECTION('center_axis',(0.,0.56333682464151,-0.826227342807548));
#10169=DIRECTION('ref_axis',(0.,0.826227342807548,0.56333682464151));
#10170=DIRECTION('',(0.,0.826227342807548,0.56333682464151));
#10171=DIRECTION('',(0.,0.826227342807548,0.56333682464151));
#10172=DIRECTION('',(1.,0.,0.));
#10173=DIRECTION('center_axis',(0.,1.,0.));
#10174=DIRECTION('ref_axis',(0.,0.,1.));
#10175=DIRECTION('',(0.,0.,1.));
#10176=DIRECTION('',(0.,0.,1.));
#10177=DIRECTION('',(1.,0.,0.));
#10178=DIRECTION('center_axis',(0.,0.56333682464151,0.826227342807548));
#10179=DIRECTION('ref_axis',(0.,-0.826227342807548,0.56333682464151));
#10180=DIRECTION('',(0.,-0.826227342807548,0.56333682464151));
#10181=DIRECTION('',(0.,-0.826227342807548,0.56333682464151));
#10182=DIRECTION('',(1.,0.,0.));
#10183=DIRECTION('center_axis',(0.,1.,0.));
#10184=DIRECTION('ref_axis',(0.,0.,1.));
#10185=DIRECTION('',(0.,0.,1.));
#10186=DIRECTION('',(0.,0.,1.));
#10187=DIRECTION('',(1.,0.,0.));
#10188=DIRECTION('center_axis',(0.,0.,-1.));
#10189=DIRECTION('ref_axis',(0.,1.,0.));
#10190=DIRECTION('',(0.,1.,0.));
#10191=DIRECTION('',(0.,1.,0.));
#10192=DIRECTION('',(1.,0.,0.));
#10193=DIRECTION('center_axis',(0.,-1.,0.));
#10194=DIRECTION('ref_axis',(0.,0.,-1.));
#10195=DIRECTION('',(0.,0.,-1.));
#10196=DIRECTION('',(0.,0.,-1.));
#10197=DIRECTION('center_axis',(1.,0.,0.));
#10198=DIRECTION('ref_axis',(0.,0.,-1.));
#10199=DIRECTION('center_axis',(1.,0.,0.));
#10200=DIRECTION('ref_axis',(0.,0.,-1.));
#10201=DIRECTION('axis',(0.,0.,1.));
#10202=DIRECTION('refdir',(1.,0.,0.));
#10203=DIRECTION('axis',(0.,0.,1.));
#10204=DIRECTION('refdir',(1.,0.,0.));
#10205=DIRECTION('center_axis',(0.,-1.,0.));
#10206=DIRECTION('ref_axis',(0.,0.,-1.));
#10207=DIRECTION('center_axis',(0.,-1.,0.));
#10208=DIRECTION('ref_axis',(1.,0.,0.));
#10209=DIRECTION('center_axis',(0.,-1.,0.));
#10210=DIRECTION('ref_axis',(1.,0.,0.));
#10211=DIRECTION('center_axis',(1.,0.,1.22464679914735E-16));
#10212=DIRECTION('ref_axis',(-1.22464679914735E-16,0.,1.));
#10213=DIRECTION('center_axis',(0.,1.,0.));
#10214=DIRECTION('ref_axis',(1.,0.,0.));
#10215=DIRECTION('center_axis',(0.,1.,0.));
#10216=DIRECTION('ref_axis',(1.,0.,0.));
#10217=DIRECTION('center_axis',(0.,-1.,0.));
#10218=DIRECTION('ref_axis',(1.,0.,0.));
#10219=DIRECTION('',(0.,1.,0.));
#10220=DIRECTION('center_axis',(0.,-1.,0.));
#10221=DIRECTION('ref_axis',(1.,0.,0.));
#10222=DIRECTION('center_axis',(0.,-1.,0.));
#10223=DIRECTION('ref_axis',(1.,0.,0.));
#10224=DIRECTION('center_axis',(0.,-1.,0.));
#10225=DIRECTION('ref_axis',(1.,0.,0.));
#10226=DIRECTION('',(0.,1.,0.));
#10227=DIRECTION('center_axis',(0.,-1.,0.));
#10228=DIRECTION('ref_axis',(1.,0.,0.));
#10229=DIRECTION('center_axis',(0.,1.,0.));
#10230=DIRECTION('ref_axis',(1.,0.,0.));
#10231=DIRECTION('',(-0.707106781186547,0.707106781186548,-8.65956056235493E-17));
#10232=DIRECTION('center_axis',(0.,-1.,0.));
#10233=DIRECTION('ref_axis',(1.,0.,0.));
#10234=DIRECTION('center_axis',(0.,1.,0.));
#10235=DIRECTION('ref_axis',(0.,0.,1.));
#10236=DIRECTION('center_axis',(0.,-1.,0.));
#10237=DIRECTION('ref_axis',(1.,0.,0.));
#10238=DIRECTION('center_axis',(0.,-1.,0.));
#10239=DIRECTION('ref_axis',(1.,0.,0.));
#10240=DIRECTION('',(0.,1.,0.));
#10241=DIRECTION('center_axis',(0.,-1.,0.));
#10242=DIRECTION('ref_axis',(0.,0.,-1.));
#10243=DIRECTION('center_axis',(0.,-1.,0.));
#10244=DIRECTION('ref_axis',(1.,0.,0.));
#10245=DIRECTION('center_axis',(0.,-1.,0.));
#10246=DIRECTION('ref_axis',(1.,0.,0.));
#10247=DIRECTION('',(0.707106781186547,0.707106781186548,8.65956056235493E-17));
#10248=DIRECTION('axis',(0.,0.,1.));
#10249=DIRECTION('refdir',(1.,0.,0.));
#10250=DIRECTION('center_axis',(0.,-1.,0.));
#10251=DIRECTION('ref_axis',(0.,0.,-1.));
#10252=DIRECTION('center_axis',(0.,-1.,0.));
#10253=DIRECTION('ref_axis',(1.,0.,0.));
#10254=DIRECTION('center_axis',(0.,-1.,0.));
#10255=DIRECTION('ref_axis',(1.,0.,0.));
#10256=DIRECTION('center_axis',(1.,0.,1.22464679914735E-16));
#10257=DIRECTION('ref_axis',(-1.22464679914735E-16,0.,1.));
#10258=DIRECTION('center_axis',(0.,1.,0.));
#10259=DIRECTION('ref_axis',(1.,0.,0.));
#10260=DIRECTION('center_axis',(0.,1.,0.));
#10261=DIRECTION('ref_axis',(1.,0.,0.));
#10262=DIRECTION('center_axis',(0.,-1.,0.));
#10263=DIRECTION('ref_axis',(1.,0.,0.));
#10264=DIRECTION('center_axis',(0.,-1.,0.));
#10265=DIRECTION('ref_axis',(1.,0.,0.));
#10266=DIRECTION('',(0.,1.,0.));
#10267=DIRECTION('center_axis',(0.,1.,0.));
#10268=DIRECTION('ref_axis',(0.,0.,1.));
#10269=DIRECTION('center_axis',(0.,-1.,0.));
#10270=DIRECTION('ref_axis',(1.,0.,0.));
#10271=DIRECTION('center_axis',(0.,-1.,0.));
#10272=DIRECTION('ref_axis',(1.,0.,0.));
#10273=DIRECTION('center_axis',(0.,-1.,0.));
#10274=DIRECTION('ref_axis',(1.,0.,0.));
#10275=DIRECTION('center_axis',(0.,-1.,0.));
#10276=DIRECTION('ref_axis',(1.,0.,0.));
#10277=DIRECTION('',(0.707106781186548,0.707106781186547,8.65956056235494E-17));
#10278=DIRECTION('center_axis',(0.,-1.,0.));
#10279=DIRECTION('ref_axis',(1.,0.,0.));
#10280=DIRECTION('center_axis',(0.,-1.,0.));
#10281=DIRECTION('ref_axis',(1.,0.,0.));
#10282=DIRECTION('',(0.,1.,0.));
#10283=DIRECTION('center_axis',(0.,1.,0.));
#10284=DIRECTION('ref_axis',(1.,0.,0.));
#10285=DIRECTION('center_axis',(0.,-1.,0.));
#10286=DIRECTION('ref_axis',(1.,0.,0.));
#10287=DIRECTION('',(-0.707106781186548,0.707106781186547,-8.65956056235494E-17));
#10288=DIRECTION('center_axis',(0.,-1.,0.));
#10289=DIRECTION('ref_axis',(0.,0.,-1.));
#10290=DIRECTION('center_axis',(0.,-1.,0.));
#10291=DIRECTION('ref_axis',(1.,0.,0.));
#10292=DIRECTION('',(0.,1.,0.));
#10293=DIRECTION('axis',(0.,0.,1.));
#10294=DIRECTION('refdir',(1.,0.,0.));
#10295=DIRECTION('center_axis',(0.,0.,1.));
#10296=DIRECTION('ref_axis',(1.,0.,0.));
#10297=DIRECTION('center_axis',(1.22464679914735E-16,-1.,0.));
#10298=DIRECTION('ref_axis',(-1.,-1.22464679914735E-16,0.));
#10299=DIRECTION('center_axis',(0.707106781186548,0.,0.707106781186548));
#10300=DIRECTION('ref_axis',(0.707106781186548,0.,-0.707106781186548));
#10301=DIRECTION('center_axis',(8.65956056235494E-17,-1.,-8.65956056235493E-17));
#10302=DIRECTION('ref_axis',(-0.707106781186547,-1.22464679914735E-16,0.707106781186547));
#10303=DIRECTION('center_axis',(1.,0.,0.));
#10304=DIRECTION('ref_axis',(6.12323399573676E-17,0.,-1.));
#10305=DIRECTION('center_axis',(7.49879891330929E-33,-1.,-1.22464679914735E-16));
#10306=DIRECTION('ref_axis',(-6.12323399573676E-17,-1.22464679914735E-16,
1.));
#10307=DIRECTION('center_axis',(0.707106781186548,0.,-0.707106781186548));
#10308=DIRECTION('ref_axis',(-0.707106781186548,0.,-0.707106781186548));
#10309=DIRECTION('center_axis',(-8.65956056235493E-17,-1.,-8.65956056235494E-17));
#10310=DIRECTION('ref_axis',(0.707106781186547,-1.22464679914735E-16,0.707106781186547));
#10311=DIRECTION('center_axis',(0.,0.,-1.));
#10312=DIRECTION('ref_axis',(-1.,0.,-1.22464679914735E-16));
#10313=DIRECTION('center_axis',(-1.22464679914735E-16,-1.,-1.49975978266186E-32));
#10314=DIRECTION('ref_axis',(1.,-1.22464679914735E-16,1.22464679914735E-16));
#10315=DIRECTION('center_axis',(-0.707106781186547,0.,-0.707106781186548));
#10316=DIRECTION('ref_axis',(-0.707106781186548,0.,0.707106781186547));
#10317=DIRECTION('center_axis',(-8.65956056235493E-17,-1.,8.65956056235493E-17));
#10318=DIRECTION('ref_axis',(0.707106781186548,-1.22464679914735E-16,-0.707106781186547));
#10319=DIRECTION('center_axis',(-1.,0.,0.));
#10320=DIRECTION('ref_axis',(-1.83697019872103E-16,0.,1.));
#10321=DIRECTION('center_axis',(-2.24963967399279E-32,-1.,1.22464679914735E-16));
#10322=DIRECTION('ref_axis',(1.83697019872103E-16,-1.22464679914735E-16,
-1.));
#10323=DIRECTION('center_axis',(-0.707106781186548,0.,0.707106781186548));
#10324=DIRECTION('ref_axis',(0.707106781186547,0.,0.707106781186548));
#10325=DIRECTION('center_axis',(8.65956056235493E-17,-1.,8.65956056235493E-17));
#10326=DIRECTION('ref_axis',(-0.707106781186547,-1.22464679914735E-16,-0.707106781186548));
#10327=DIRECTION('axis',(0.,0.,1.));
#10328=DIRECTION('refdir',(1.,0.,0.));
#10329=DIRECTION('center_axis',(0.,0.,1.));
#10330=DIRECTION('ref_axis',(1.,0.,0.));
#10331=DIRECTION('center_axis',(0.,-1.,0.));
#10332=DIRECTION('ref_axis',(0.,0.,-1.));
#10333=DIRECTION('center_axis',(0.,-1.,0.));
#10334=DIRECTION('ref_axis',(0.,0.,-1.));
#10335=DIRECTION('center_axis',(0.,1.,0.));
#10336=DIRECTION('ref_axis',(1.,0.,0.));
#10337=DIRECTION('center_axis',(0.,1.,0.));
#10338=DIRECTION('ref_axis',(1.,0.,0.));
#10339=DIRECTION('center_axis',(0.,1.,0.));
#10340=DIRECTION('ref_axis',(1.,0.,0.));
#10341=DIRECTION('center_axis',(0.,1.,0.));
#10342=DIRECTION('ref_axis',(1.,0.,0.));
#10343=DIRECTION('',(0.,-1.,0.));
#10344=DIRECTION('center_axis',(0.,-1.,0.));
#10345=DIRECTION('ref_axis',(1.,0.,0.));
#10346=DIRECTION('center_axis',(0.,1.,0.));
#10347=DIRECTION('ref_axis',(1.,0.,0.));
#10348=DIRECTION('center_axis',(0.,1.,0.));
#10349=DIRECTION('ref_axis',(1.,0.,0.));
#10350=DIRECTION('center_axis',(0.,1.,0.));
#10351=DIRECTION('ref_axis',(1.,0.,0.));
#10352=DIRECTION('center_axis',(0.,1.,0.));
#10353=DIRECTION('ref_axis',(1.,0.,0.));
#10354=DIRECTION('center_axis',(0.,1.,0.));
#10355=DIRECTION('ref_axis',(1.,0.,0.));
#10356=DIRECTION('center_axis',(0.,1.,0.));
#10357=DIRECTION('ref_axis',(1.,0.,0.));
#10358=DIRECTION('center_axis',(0.,-1.,0.));
#10359=DIRECTION('ref_axis',(1.,0.,0.));
#10360=DIRECTION('center_axis',(0.,-1.,0.));
#10361=DIRECTION('ref_axis',(0.,0.,-1.));
#10362=DIRECTION('center_axis',(6.12323399573677E-17,0.,1.));
#10363=DIRECTION('ref_axis',(1.,0.,0.));
#10364=DIRECTION('center_axis',(0.,-1.,0.));
#10365=DIRECTION('ref_axis',(0.,0.,-1.));
#10366=DIRECTION('center_axis',(0.,1.,0.));
#10367=DIRECTION('ref_axis',(1.,0.,0.));
#10368=DIRECTION('center_axis',(0.,-1.,0.));
#10369=DIRECTION('ref_axis',(1.,0.,0.));
#10370=DIRECTION('center_axis',(0.,-1.,0.));
#10371=DIRECTION('ref_axis',(0.,0.,-1.));
#10372=DIRECTION('center_axis',(0.,0.,1.));
#10373=DIRECTION('ref_axis',(1.,0.,0.));
#10374=DIRECTION('center_axis',(0.,-1.,0.));
#10375=DIRECTION('ref_axis',(0.,0.,-1.));
#10376=DIRECTION('center_axis',(0.,1.,0.));
#10377=DIRECTION('ref_axis',(1.,0.,0.));
#10378=DIRECTION('center_axis',(0.,-1.,0.));
#10379=DIRECTION('ref_axis',(1.,0.,0.));
#10380=DIRECTION('center_axis',(0.,-1.,0.));
#10381=DIRECTION('ref_axis',(0.,0.,-1.));
#10382=DIRECTION('center_axis',(0.,0.,1.));
#10383=DIRECTION('ref_axis',(1.,0.,0.));
#10384=DIRECTION('center_axis',(0.,-1.,0.));
#10385=DIRECTION('ref_axis',(0.,0.,-1.));
#10386=DIRECTION('center_axis',(0.,1.,0.));
#10387=DIRECTION('ref_axis',(1.,0.,0.));
#10388=DIRECTION('center_axis',(0.,-1.,0.));
#10389=DIRECTION('ref_axis',(1.,0.,0.));
#10390=DIRECTION('center_axis',(0.,-1.,0.));
#10391=DIRECTION('ref_axis',(0.,0.,-1.));
#10392=DIRECTION('center_axis',(0.,0.,1.));
#10393=DIRECTION('ref_axis',(1.,0.,0.));
#10394=DIRECTION('center_axis',(0.,-1.,0.));
#10395=DIRECTION('ref_axis',(0.,0.,-1.));
#10396=DIRECTION('center_axis',(0.,1.,0.));
#10397=DIRECTION('ref_axis',(1.,0.,0.));
#10398=DIRECTION('center_axis',(0.,-1.,0.));
#10399=DIRECTION('ref_axis',(1.,0.,0.));
#10400=DIRECTION('center_axis',(0.,-1.,0.));
#10401=DIRECTION('ref_axis',(0.,0.,-1.));
#10402=DIRECTION('center_axis',(6.12323399573676E-17,0.,1.));
#10403=DIRECTION('ref_axis',(1.,0.,0.));
#10404=DIRECTION('center_axis',(0.,-1.,0.));
#10405=DIRECTION('ref_axis',(0.,0.,-1.));
#10406=DIRECTION('center_axis',(0.,1.,0.));
#10407=DIRECTION('ref_axis',(1.,0.,0.));
#10408=DIRECTION('center_axis',(0.,-1.,0.));
#10409=DIRECTION('ref_axis',(1.,0.,0.));
#10410=DIRECTION('center_axis',(0.,-1.,0.));
#10411=DIRECTION('ref_axis',(0.,0.,-1.));
#10412=DIRECTION('center_axis',(0.,0.,1.));
#10413=DIRECTION('ref_axis',(1.,0.,0.));
#10414=DIRECTION('center_axis',(0.,-1.,0.));
#10415=DIRECTION('ref_axis',(0.,0.,-1.));
#10416=DIRECTION('center_axis',(0.,1.,0.));
#10417=DIRECTION('ref_axis',(1.,0.,0.));
#10418=DIRECTION('center_axis',(0.,1.,0.));
#10419=DIRECTION('ref_axis',(1.,0.,0.));
#10420=DIRECTION('',(0.,1.,0.));
#10421=DIRECTION('center_axis',(0.,-1.,0.));
#10422=DIRECTION('ref_axis',(1.,0.,0.));
#10423=DIRECTION('center_axis',(0.,-1.,0.));
#10424=DIRECTION('ref_axis',(1.,0.,0.));
#10425=DIRECTION('center_axis',(0.,1.,0.));
#10426=DIRECTION('ref_axis',(1.,0.,0.));
#10427=DIRECTION('center_axis',(0.,-1.,0.));
#10428=DIRECTION('ref_axis',(0.,0.,-1.));
#10429=DIRECTION('center_axis',(0.,0.,1.));
#10430=DIRECTION('ref_axis',(1.,0.,0.));
#10431=DIRECTION('center_axis',(0.,-1.,0.));
#10432=DIRECTION('ref_axis',(0.,0.,-1.));
#10433=DIRECTION('center_axis',(0.,-1.,0.));
#10434=DIRECTION('ref_axis',(-1.,0.,0.));
#10435=DIRECTION('center_axis',(0.,1.,0.));
#10436=DIRECTION('ref_axis',(1.,0.,0.));
#10437=DIRECTION('axis',(0.,0.,1.));
#10438=DIRECTION('refdir',(1.,0.,0.));
#10439=DIRECTION('center_axis',(0.,1.,0.));
#10440=DIRECTION('ref_axis',(0.,0.,1.));
#10441=DIRECTION('center_axis',(0.,-1.,0.));
#10442=DIRECTION('ref_axis',(1.,0.,0.));
#10443=DIRECTION('center_axis',(0.,-1.,0.));
#10444=DIRECTION('ref_axis',(1.,0.,0.));
#10445=DIRECTION('center_axis',(0.,-1.,0.));
#10446=DIRECTION('ref_axis',(1.,0.,0.));
#10447=DIRECTION('center_axis',(0.,-1.,0.));
#10448=DIRECTION('ref_axis',(1.,0.,0.));
#10449=DIRECTION('',(0.,1.,0.));
#10450=DIRECTION('center_axis',(0.,-1.,0.));
#10451=DIRECTION('ref_axis',(0.,0.,-1.));
#10452=DIRECTION('center_axis',(0.,-1.,0.));
#10453=DIRECTION('ref_axis',(1.,0.,0.));
#10454=DIRECTION('center_axis',(0.,-1.,0.));
#10455=DIRECTION('ref_axis',(1.,0.,0.));
#10456=DIRECTION('',(0.,1.,0.));
#10457=DIRECTION('center_axis',(0.,1.,0.));
#10458=DIRECTION('ref_axis',(0.,0.,1.));
#10459=DIRECTION('center_axis',(0.,-1.,0.));
#10460=DIRECTION('ref_axis',(1.,0.,0.));
#10461=DIRECTION('center_axis',(0.,-1.,0.));
#10462=DIRECTION('ref_axis',(1.,0.,0.));
#10463=DIRECTION('center_axis',(0.,-1.,0.));
#10464=DIRECTION('ref_axis',(1.,0.,0.));
#10465=DIRECTION('center_axis',(0.,-1.,0.));
#10466=DIRECTION('ref_axis',(1.,0.,0.));
#10467=DIRECTION('',(0.,1.,0.));
#10468=DIRECTION('center_axis',(0.,-1.,0.));
#10469=DIRECTION('ref_axis',(0.,0.,-1.));
#10470=DIRECTION('center_axis',(0.,-1.,0.));
#10471=DIRECTION('ref_axis',(1.,0.,0.));
#10472=DIRECTION('center_axis',(0.,-1.,0.));
#10473=DIRECTION('ref_axis',(1.,0.,0.));
#10474=DIRECTION('',(0.,1.,0.));
#10475=DIRECTION('',(0.,0.,1.));
#10476=DIRECTION('',(1.,0.,0.));
#10477=DIRECTION('',(0.,0.,1.));
#10478=DIRECTION('',(1.,0.,0.));
#10479=DIRECTION('',(0.,0.,1.));
#10480=DIRECTION('',(1.,0.,0.));
#10481=DIRECTION('',(0.,0.,1.));
#10482=DIRECTION('',(1.,0.,0.));
#10483=DIRECTION('',(0.,0.,1.));
#10484=DIRECTION('',(1.,0.,0.));
#10485=DIRECTION('axis',(0.,0.,1.));
#10486=DIRECTION('refdir',(1.,0.,0.));
#10487=DIRECTION('axis',(0.,0.,1.));
#10488=DIRECTION('refdir',(1.,0.,0.));
#10489=DIRECTION('center_axis',(0.,0.,1.));
#10490=DIRECTION('ref_axis',(1.,0.,0.));
#10491=DIRECTION('center_axis',(0.,0.,1.));
#10492=DIRECTION('ref_axis',(1.,0.,0.));
#10493=DIRECTION('',(0.,0.,1.));
#10494=DIRECTION('center_axis',(0.,0.,-1.));
#10495=DIRECTION('ref_axis',(1.,0.,0.));
#10496=DIRECTION('center_axis',(0.,0.,1.));
#10497=DIRECTION('ref_axis',(-1.,-1.22464679914735E-16,0.));
#10498=DIRECTION('',(0.,0.,-1.));
#10499=DIRECTION('center_axis',(0.,0.,1.));
#10500=DIRECTION('ref_axis',(1.,0.,0.));
#10501=DIRECTION('',(0.,0.,1.));
#10502=DIRECTION('center_axis',(0.,0.,1.));
#10503=DIRECTION('ref_axis',(1.,0.,0.));
#10504=DIRECTION('center_axis',(0.,-1.,0.));
#10505=DIRECTION('ref_axis',(1.,0.,0.));
#10506=DIRECTION('',(-1.,0.,0.));
#10507=DIRECTION('',(0.,0.,-1.));
#10508=DIRECTION('',(1.,0.,0.));
#10509=DIRECTION('center_axis',(0.,0.,1.));
#10510=DIRECTION('ref_axis',(1.,0.,0.));
#10511=DIRECTION('',(1.,0.,0.));
#10512=DIRECTION('center_axis',(0.,0.,1.));
#10513=DIRECTION('ref_axis',(1.,0.,0.));
#10514=DIRECTION('',(0.,1.,0.));
#10515=DIRECTION('center_axis',(0.,0.,1.));
#10516=DIRECTION('ref_axis',(1.,0.,0.));
#10517=DIRECTION('',(0.,-1.,0.));
#10518=DIRECTION('center_axis',(0.,0.,1.));
#10519=DIRECTION('ref_axis',(1.,0.,0.));
#10520=DIRECTION('center_axis',(0.,0.,1.));
#10521=DIRECTION('ref_axis',(1.,0.,0.));
#10522=DIRECTION('center_axis',(0.,0.,1.));
#10523=DIRECTION('ref_axis',(1.,0.,0.));
#10524=DIRECTION('center_axis',(0.,1.,0.));
#10525=DIRECTION('ref_axis',(-1.,0.,0.));
#10526=DIRECTION('',(-1.,0.,0.));
#10527=DIRECTION('',(0.,0.,1.));
#10528=DIRECTION('center_axis',(0.,0.,1.));
#10529=DIRECTION('ref_axis',(1.,0.,0.));
#10530=DIRECTION('center_axis',(0.,0.,1.));
#10531=DIRECTION('ref_axis',(1.,0.,0.));
#10532=DIRECTION('',(0.,0.,-1.));
#10533=DIRECTION('center_axis',(0.,0.,1.));
#10534=DIRECTION('ref_axis',(1.,0.,0.));
#10535=DIRECTION('',(0.,0.,1.));
#10536=DIRECTION('center_axis',(0.,0.,-1.));
#10537=DIRECTION('ref_axis',(1.,0.,0.));
#10538=DIRECTION('center_axis',(0.,0.,1.));
#10539=DIRECTION('ref_axis',(6.12323399573677E-17,1.,0.));
#10540=DIRECTION('',(0.,0.,1.));
#10541=DIRECTION('',(0.,0.,-1.));
#10542=DIRECTION('center_axis',(0.,0.,1.));
#10543=DIRECTION('ref_axis',(1.,0.,0.));
#10544=DIRECTION('center_axis',(1.,0.,0.));
#10545=DIRECTION('ref_axis',(0.,1.,0.));
#10546=DIRECTION('',(0.,1.,0.));
#10547=DIRECTION('',(0.,0.,1.));
#10548=DIRECTION('center_axis',(0.,0.,1.));
#10549=DIRECTION('ref_axis',(1.,0.,0.));
#10550=DIRECTION('center_axis',(0.,0.,1.));
#10551=DIRECTION('ref_axis',(1.,0.,0.));
#10552=DIRECTION('',(0.,-1.,0.));
#10553=DIRECTION('center_axis',(-1.,0.,0.));
#10554=DIRECTION('ref_axis',(0.,-1.,0.));
#10555=DIRECTION('center_axis',(0.,0.,1.));
#10556=DIRECTION('ref_axis',(1.,0.,0.));
#10557=DIRECTION('center_axis',(0.,0.,1.));
#10558=DIRECTION('ref_axis',(1.,0.,0.));
#10559=DIRECTION('center_axis',(0.,0.,1.));
#10560=DIRECTION('ref_axis',(1.,0.,0.));
#10561=DIRECTION('center_axis',(0.,0.,-1.));
#10562=DIRECTION('ref_axis',(1.,0.,0.));
#10563=DIRECTION('center_axis',(0.,0.,1.));
#10564=DIRECTION('ref_axis',(1.,0.,0.));
#10565=DIRECTION('',(0.,0.,-1.));
#10566=DIRECTION('center_axis',(0.,0.,1.));
#10567=DIRECTION('ref_axis',(1.,0.,0.));
#10568=DIRECTION('',(0.,0.,-1.));
#10569=DIRECTION('center_axis',(0.,0.,1.));
#10570=DIRECTION('ref_axis',(1.,0.,0.));
#10571=DIRECTION('center_axis',(0.,0.,1.));
#10572=DIRECTION('ref_axis',(1.,0.,0.));
#10573=DIRECTION('axis',(0.,0.,1.));
#10574=DIRECTION('refdir',(1.,0.,0.));
#10575=DIRECTION('center_axis',(0.,0.,1.));
#10576=DIRECTION('ref_axis',(1.,0.,0.));
#10577=DIRECTION('center_axis',(0.,0.,1.));
#10578=DIRECTION('ref_axis',(1.,0.,0.));
#10579=DIRECTION('',(0.,0.,1.));
#10580=DIRECTION('center_axis',(0.,0.,-1.));
#10581=DIRECTION('ref_axis',(1.,0.,0.));
#10582=DIRECTION('center_axis',(0.,0.,1.));
#10583=DIRECTION('ref_axis',(1.,0.,0.));
#10584=DIRECTION('center_axis',(0.,0.,1.));
#10585=DIRECTION('ref_axis',(1.,0.,0.));
#10586=DIRECTION('center_axis',(0.,0.,1.));
#10587=DIRECTION('ref_axis',(1.,0.,0.));
#10588=DIRECTION('',(0.,0.,-1.));
#10589=DIRECTION('center_axis',(0.,0.,1.));
#10590=DIRECTION('ref_axis',(1.,0.,0.));
#10591=DIRECTION('center_axis',(0.,0.,1.));
#10592=DIRECTION('ref_axis',(1.,0.,0.));
#10593=DIRECTION('center_axis',(0.,0.,1.));
#10594=DIRECTION('ref_axis',(1.,0.,0.));
#10595=DIRECTION('axis',(0.,0.,1.));
#10596=DIRECTION('refdir',(1.,0.,0.));
#10597=DIRECTION('center_axis',(0.,0.,1.));
#10598=DIRECTION('ref_axis',(1.,0.,0.));
#10599=DIRECTION('center_axis',(0.,0.,-1.));
#10600=DIRECTION('ref_axis',(1.,0.,0.));
#10601=DIRECTION('',(0.,0.,-1.));
#10602=DIRECTION('center_axis',(0.,0.,-1.));
#10603=DIRECTION('ref_axis',(1.,0.,0.));
#10604=DIRECTION('center_axis',(0.,0.,1.));
#10605=DIRECTION('ref_axis',(1.,0.,0.));
#10606=DIRECTION('center_axis',(0.,0.,1.));
#10607=DIRECTION('ref_axis',(1.,0.,0.));
#10608=DIRECTION('',(0.,0.,-1.));
#10609=DIRECTION('center_axis',(0.,0.,1.));
#10610=DIRECTION('ref_axis',(1.,0.,0.));
#10611=DIRECTION('center_axis',(0.,0.,1.));
#10612=DIRECTION('ref_axis',(1.,0.,0.));
#10613=DIRECTION('center_axis',(0.,0.,1.));
#10614=DIRECTION('ref_axis',(1.,0.,0.));
#10615=DIRECTION('axis',(0.,0.,1.));
#10616=DIRECTION('refdir',(1.,0.,0.));
#10617=DIRECTION('center_axis',(1.,0.,0.));
#10618=DIRECTION('ref_axis',(0.,0.,-1.));
#10619=DIRECTION('',(0.,0.,1.));
#10620=DIRECTION('center_axis',(1.,0.,0.));
#10621=DIRECTION('ref_axis',(0.,0.,-1.));
#10622=DIRECTION('center_axis',(1.,0.,0.));
#10623=DIRECTION('ref_axis',(0.,0.,-1.));
#10624=DIRECTION('center_axis',(1.,0.,0.));
#10625=DIRECTION('ref_axis',(0.,0.,-1.));
#10626=DIRECTION('',(1.,0.,0.));
#10627=DIRECTION('center_axis',(1.,0.,0.));
#10628=DIRECTION('ref_axis',(0.,0.,-1.));
#10629=DIRECTION('',(0.,0.,-1.));
#10630=DIRECTION('center_axis',(0.,0.,1.));
#10631=DIRECTION('ref_axis',(1.,0.,0.));
#10632=DIRECTION('center_axis',(0.,0.,-1.));
#10633=DIRECTION('ref_axis',(1.,0.,0.));
#10634=DIRECTION('',(0.,0.,-1.));
#10635=DIRECTION('center_axis',(0.,0.,-1.));
#10636=DIRECTION('ref_axis',(1.,0.,0.));
#10637=DIRECTION('center_axis',(0.,0.,1.));
#10638=DIRECTION('ref_axis',(1.,0.,0.));
#10639=DIRECTION('center_axis',(0.,0.,1.));
#10640=DIRECTION('ref_axis',(1.,0.,0.));
#10641=DIRECTION('',(0.,0.,-1.));
#10642=DIRECTION('center_axis',(0.,0.,1.));
#10643=DIRECTION('ref_axis',(1.,0.,0.));
#10644=DIRECTION('center_axis',(0.,0.,1.));
#10645=DIRECTION('ref_axis',(1.,0.,0.));
#10646=DIRECTION('center_axis',(0.,0.,1.));
#10647=DIRECTION('ref_axis',(1.,0.,0.));
#10648=DIRECTION('axis',(0.,0.,1.));
#10649=DIRECTION('refdir',(1.,0.,0.));
#10650=DIRECTION('center_axis',(0.,0.,1.));
#10651=DIRECTION('ref_axis',(1.,0.,0.));
#10652=DIRECTION('center_axis',(0.,0.,1.));
#10653=DIRECTION('ref_axis',(1.,0.,0.));
#10654=DIRECTION('',(0.,0.,1.));
#10655=DIRECTION('center_axis',(0.,0.,-1.));
#10656=DIRECTION('ref_axis',(1.,0.,0.));
#10657=DIRECTION('center_axis',(0.,0.,1.));
#10658=DIRECTION('ref_axis',(1.,0.,0.));
#10659=DIRECTION('center_axis',(0.,0.,1.));
#10660=DIRECTION('ref_axis',(1.,0.,0.));
#10661=DIRECTION('center_axis',(0.,0.,1.));
#10662=DIRECTION('ref_axis',(1.,0.,0.));
#10663=DIRECTION('center_axis',(0.,0.,1.));
#10664=DIRECTION('ref_axis',(1.,0.,0.));
#10665=DIRECTION('center_axis',(0.,0.,1.));
#10666=DIRECTION('ref_axis',(1.,0.,0.));
#10667=DIRECTION('center_axis',(0.,0.,1.));
#10668=DIRECTION('ref_axis',(1.,0.,0.));
#10669=DIRECTION('center_axis',(0.,0.,-1.));
#10670=DIRECTION('ref_axis',(1.,0.,0.));
#10671=DIRECTION('center_axis',(0.,0.,1.));
#10672=DIRECTION('ref_axis',(1.,0.,0.));
#10673=DIRECTION('',(0.,0.,-1.));
#10674=DIRECTION('center_axis',(0.,0.,1.));
#10675=DIRECTION('ref_axis',(1.,0.,0.));
#10676=DIRECTION('',(0.,0.,-1.));
#10677=DIRECTION('center_axis',(0.,0.,1.));
#10678=DIRECTION('ref_axis',(1.,0.,0.));
#10679=DIRECTION('center_axis',(0.,0.,1.));
#10680=DIRECTION('ref_axis',(1.,0.,0.));
#10681=DIRECTION('center_axis',(0.,0.,1.));
#10682=DIRECTION('ref_axis',(1.,0.,0.));
#10683=DIRECTION('',(0.,0.,-1.));
#10684=DIRECTION('center_axis',(0.,0.,1.));
#10685=DIRECTION('ref_axis',(1.,0.,0.));
#10686=DIRECTION('center_axis',(0.,0.,1.));
#10687=DIRECTION('ref_axis',(1.,0.,0.));
#10688=DIRECTION('axis',(0.,0.,1.));
#10689=DIRECTION('refdir',(1.,0.,0.));
#10690=DIRECTION('center_axis',(0.,0.,1.));
#10691=DIRECTION('ref_axis',(1.,0.,0.));
#10692=DIRECTION('center_axis',(0.,0.,-1.));
#10693=DIRECTION('ref_axis',(1.,0.,0.));
#10694=DIRECTION('',(0.,0.,-1.));
#10695=DIRECTION('center_axis',(0.,0.,-1.));
#10696=DIRECTION('ref_axis',(1.,0.,0.));
#10697=DIRECTION('center_axis',(0.,0.,1.));
#10698=DIRECTION('ref_axis',(1.,0.,0.));
#10699=DIRECTION('center_axis',(0.,0.,1.));
#10700=DIRECTION('ref_axis',(1.,0.,0.));
#10701=DIRECTION('',(0.,0.,-1.));
#10702=DIRECTION('center_axis',(0.,0.,1.));
#10703=DIRECTION('ref_axis',(1.,0.,0.));
#10704=DIRECTION('center_axis',(0.,0.,1.));
#10705=DIRECTION('ref_axis',(1.,0.,0.));
#10706=DIRECTION('center_axis',(0.,0.,1.));
#10707=DIRECTION('ref_axis',(1.,0.,0.));
#10708=DIRECTION('axis',(0.,0.,1.));
#10709=DIRECTION('refdir',(1.,0.,0.));
#10710=DIRECTION('center_axis',(0.,0.,1.));
#10711=DIRECTION('ref_axis',(1.,0.,0.));
#10712=DIRECTION('center_axis',(0.,0.,-1.));
#10713=DIRECTION('ref_axis',(1.,0.,0.));
#10714=DIRECTION('',(0.,0.,-1.));
#10715=DIRECTION('center_axis',(0.,0.,-1.));
#10716=DIRECTION('ref_axis',(1.,0.,0.));
#10717=DIRECTION('center_axis',(0.,0.,1.));
#10718=DIRECTION('ref_axis',(1.,0.,0.));
#10719=DIRECTION('center_axis',(0.,0.,1.));
#10720=DIRECTION('ref_axis',(1.,0.,0.));
#10721=DIRECTION('',(0.,0.,-1.));
#10722=DIRECTION('center_axis',(0.,0.,1.));
#10723=DIRECTION('ref_axis',(1.,0.,0.));
#10724=DIRECTION('center_axis',(0.,0.,1.));
#10725=DIRECTION('ref_axis',(1.,0.,0.));
#10726=DIRECTION('center_axis',(0.,0.,1.));
#10727=DIRECTION('ref_axis',(1.,0.,0.));
#10728=DIRECTION('axis',(0.,0.,1.));
#10729=DIRECTION('refdir',(1.,0.,0.));
#10730=DIRECTION('center_axis',(0.,0.,1.));
#10731=DIRECTION('ref_axis',(1.,0.,0.));
#10732=DIRECTION('center_axis',(0.,0.,-1.));
#10733=DIRECTION('ref_axis',(1.,0.,0.));
#10734=DIRECTION('',(0.,0.,-1.));
#10735=DIRECTION('center_axis',(0.,0.,-1.));
#10736=DIRECTION('ref_axis',(1.,0.,0.));
#10737=DIRECTION('center_axis',(0.,0.,1.));
#10738=DIRECTION('ref_axis',(1.,0.,0.));
#10739=DIRECTION('center_axis',(0.,0.,1.));
#10740=DIRECTION('ref_axis',(1.,0.,0.));
#10741=DIRECTION('',(0.,0.,-1.));
#10742=DIRECTION('center_axis',(0.,0.,1.));
#10743=DIRECTION('ref_axis',(1.,0.,0.));
#10744=DIRECTION('center_axis',(0.,0.,1.));
#10745=DIRECTION('ref_axis',(1.,0.,0.));
#10746=DIRECTION('center_axis',(0.,0.,1.));
#10747=DIRECTION('ref_axis',(1.,0.,0.));
#10748=DIRECTION('axis',(0.,0.,1.));
#10749=DIRECTION('refdir',(1.,0.,0.));
#10750=DIRECTION('center_axis',(0.,1.,0.));
#10751=DIRECTION('ref_axis',(0.,0.,1.));
#10752=DIRECTION('center_axis',(0.,-1.,0.));
#10753=DIRECTION('ref_axis',(1.,0.,0.));
#10754=DIRECTION('center_axis',(0.,-1.,0.));
#10755=DIRECTION('ref_axis',(1.,0.,0.));
#10756=DIRECTION('center_axis',(0.,-1.,0.));
#10757=DIRECTION('ref_axis',(1.,0.,0.));
#10758=DIRECTION('',(0.707106781186547,0.707106781186548,8.65956056235493E-17));
#10759=DIRECTION('center_axis',(0.,-1.,0.));
#10760=DIRECTION('ref_axis',(1.,0.,0.));
#10761=DIRECTION('center_axis',(0.,-1.,0.));
#10762=DIRECTION('ref_axis',(1.,0.,0.));
#10763=DIRECTION('',(0.,1.,0.));
#10764=DIRECTION('center_axis',(0.,1.,0.));
#10765=DIRECTION('ref_axis',(1.,0.,0.));
#10766=DIRECTION('center_axis',(0.,-1.,0.));
#10767=DIRECTION('ref_axis',(1.,0.,0.));
#10768=DIRECTION('',(-0.707106781186547,0.707106781186548,-8.65956056235493E-17));
#10769=DIRECTION('center_axis',(0.,-1.,0.));
#10770=DIRECTION('ref_axis',(0.,0.,-1.));
#10771=DIRECTION('center_axis',(0.,-1.,0.));
#10772=DIRECTION('ref_axis',(1.,0.,0.));
#10773=DIRECTION('center_axis',(0.,1.,0.));
#10774=DIRECTION('ref_axis',(1.,0.,0.));
#10775=DIRECTION('center_axis',(0.,1.,0.));
#10776=DIRECTION('ref_axis',(1.,0.,0.));
#10777=DIRECTION('',(-0.447213595499958,0.894427190999916,-5.47678698264203E-17));
#10778=DIRECTION('center_axis',(0.,-1.,0.));
#10779=DIRECTION('ref_axis',(1.,0.,0.));
#10780=DIRECTION('center_axis',(0.,1.,0.));
#10781=DIRECTION('ref_axis',(1.,0.,0.));
#10782=DIRECTION('',(0.,1.,0.));
#10783=DIRECTION('center_axis',(0.,1.,0.));
#10784=DIRECTION('ref_axis',(1.,0.,0.));
#10785=DIRECTION('center_axis',(0.,-1.,0.));
#10786=DIRECTION('ref_axis',(1.,0.,0.));
#10787=DIRECTION('',(-0.707106781186547,0.707106781186548,-8.65956056235493E-17));
#10788=DIRECTION('center_axis',(0.,-1.,0.));
#10789=DIRECTION('ref_axis',(0.,0.,-1.));
#10790=DIRECTION('center_axis',(0.866025403784439,0.,-0.5));
#10791=DIRECTION('ref_axis',(0.5,0.,0.866025403784439));
#10792=DIRECTION('',(-0.5,0.,-0.866025403784439));
#10793=DIRECTION('',(0.,-1.,0.));
#10794=DIRECTION('',(0.5,0.,0.866025403784439));
#10795=DIRECTION('',(0.,-1.,0.));
#10796=DIRECTION('center_axis',(1.60246890531964E-16,0.,-1.));
#10797=DIRECTION('ref_axis',(1.,0.,1.60246890531964E-16));
#10798=DIRECTION('',(-1.,0.,-1.60246890531964E-16));
#10799=DIRECTION('',(0.,-1.,0.));
#10800=DIRECTION('',(1.,0.,1.60246890531964E-16));
#10801=DIRECTION('center_axis',(-0.866025403784439,0.,-0.5));
#10802=DIRECTION('ref_axis',(0.5,0.,-0.866025403784439));
#10803=DIRECTION('',(-0.5,0.,0.866025403784439));
#10804=DIRECTION('',(0.,-1.,0.));
#10805=DIRECTION('',(0.5,0.,-0.866025403784439));
#10806=DIRECTION('center_axis',(-0.866025403784439,0.,0.5));
#10807=DIRECTION('ref_axis',(-0.5,0.,-0.866025403784439));
#10808=DIRECTION('',(0.5,0.,0.866025403784439));
#10809=DIRECTION('',(0.,-1.,0.));
#10810=DIRECTION('',(-0.5,0.,-0.866025403784439));
#10811=DIRECTION('center_axis',(-1.60246890531964E-16,0.,1.));
#10812=DIRECTION('ref_axis',(-1.,0.,-1.60246890531964E-16));
#10813=DIRECTION('',(1.,0.,1.60246890531964E-16));
#10814=DIRECTION('',(0.,-1.,0.));
#10815=DIRECTION('',(-1.,0.,-1.60246890531964E-16));
#10816=DIRECTION('center_axis',(0.866025403784439,0.,0.5));
#10817=DIRECTION('ref_axis',(-0.5,0.,0.866025403784439));
#10818=DIRECTION('',(0.5,0.,-0.866025403784439));
#10819=DIRECTION('',(-0.5,0.,0.866025403784439));
#10820=DIRECTION('center_axis',(0.,1.,0.));
#10821=DIRECTION('ref_axis',(1.,0.,0.));
#10822=DIRECTION('center_axis',(0.,-1.,0.));
#10823=DIRECTION('ref_axis',(0.,0.,-1.));
#10824=DIRECTION('axis',(0.,0.,1.));
#10825=DIRECTION('refdir',(1.,0.,0.));
#10826=DIRECTION('axis',(0.,0.,1.));
#10827=DIRECTION('refdir',(1.,0.,0.));
#10828=DIRECTION('center_axis',(0.,0.,1.));
#10829=DIRECTION('ref_axis',(1.,0.,0.));
#10830=DIRECTION('center_axis',(0.,0.,1.));
#10831=DIRECTION('ref_axis',(1.,0.,0.));
#10832=DIRECTION('',(0.,0.,1.));
#10833=DIRECTION('center_axis',(0.,0.,-1.));
#10834=DIRECTION('ref_axis',(1.,0.,0.));
#10835=DIRECTION('center_axis',(0.,-1.,0.));
#10836=DIRECTION('ref_axis',(1.,0.,0.));
#10837=DIRECTION('',(1.,0.,0.));
#10838=DIRECTION('',(0.,0.,1.));
#10839=DIRECTION('',(-1.,0.,0.));
#10840=DIRECTION('',(0.,0.,1.));
#10841=DIRECTION('center_axis',(1.,0.,0.));
#10842=DIRECTION('ref_axis',(0.,1.,0.));
#10843=DIRECTION('',(0.,1.,0.));
#10844=DIRECTION('',(0.,-1.,0.));
#10845=DIRECTION('',(0.,0.,1.));
#10846=DIRECTION('center_axis',(0.,1.,0.));
#10847=DIRECTION('ref_axis',(-1.,0.,0.));
#10848=DIRECTION('',(-1.,0.,0.));
#10849=DIRECTION('',(1.,0.,0.));
#10850=DIRECTION('',(0.,0.,1.));
#10851=DIRECTION('center_axis',(-1.,0.,0.));
#10852=DIRECTION('ref_axis',(0.,-1.,0.));
#10853=DIRECTION('',(0.,-1.,0.));
#10854=DIRECTION('',(0.,1.,0.));
#10855=DIRECTION('center_axis',(0.,0.,1.));
#10856=DIRECTION('ref_axis',(1.,0.,0.));
#10857=DIRECTION('',(0.,0.,1.));
#10858=DIRECTION('center_axis',(0.,0.,1.));
#10859=DIRECTION('ref_axis',(1.,0.,0.));
#10860=DIRECTION('',(0.,0.,1.));
#10861=DIRECTION('center_axis',(0.,0.,1.));
#10862=DIRECTION('ref_axis',(1.,0.,0.));
#10863=DIRECTION('center_axis',(0.,0.,1.));
#10864=DIRECTION('ref_axis',(1.,0.,0.));
#10865=DIRECTION('',(0.,-1.,0.));
#10866=DIRECTION('center_axis',(0.,0.,1.));
#10867=DIRECTION('ref_axis',(1.,0.,0.));
#10868=DIRECTION('',(0.,1.,0.));
#10869=DIRECTION('center_axis',(0.,0.,1.));
#10870=DIRECTION('ref_axis',(1.,0.,0.));
#10871=DIRECTION('center_axis',(-1.,0.,0.));
#10872=DIRECTION('ref_axis',(0.,-1.,0.));
#10873=DIRECTION('',(0.,0.,-1.));
#10874=DIRECTION('',(0.,-1.,0.));
#10875=DIRECTION('center_axis',(1.,0.,0.));
#10876=DIRECTION('ref_axis',(0.,1.,0.));
#10877=DIRECTION('',(0.,1.,0.));
#10878=DIRECTION('',(0.,0.,1.));
#10879=DIRECTION('center_axis',(0.,0.,1.));
#10880=DIRECTION('ref_axis',(1.,0.,0.));
#10881=DIRECTION('center_axis',(0.,0.,1.));
#10882=DIRECTION('ref_axis',(1.,0.,0.));
#10883=DIRECTION('center_axis',(0.,0.,1.));
#10884=DIRECTION('ref_axis',(1.,0.,0.));
#10885=DIRECTION('center_axis',(0.,0.,1.));
#10886=DIRECTION('ref_axis',(1.,0.,0.));
#10887=DIRECTION('center_axis',(0.,0.,-1.));
#10888=DIRECTION('ref_axis',(1.,0.,0.));
#10889=DIRECTION('center_axis',(0.,0.,1.));
#10890=DIRECTION('ref_axis',(1.,0.,0.));
#10891=DIRECTION('',(0.,0.,-1.));
#10892=DIRECTION('center_axis',(0.,0.,1.));
#10893=DIRECTION('ref_axis',(1.,0.,0.));
#10894=DIRECTION('',(0.,0.,-1.));
#10895=DIRECTION('center_axis',(0.,0.,1.));
#10896=DIRECTION('ref_axis',(1.,0.,0.));
#10897=DIRECTION('center_axis',(0.,0.,1.));
#10898=DIRECTION('ref_axis',(1.,0.,0.));
#10899=DIRECTION('center_axis',(0.,0.,1.));
#10900=DIRECTION('ref_axis',(1.,0.,0.));
#10901=DIRECTION('axis',(0.,0.,1.));
#10902=DIRECTION('refdir',(1.,0.,0.));
#10903=DIRECTION('center_axis',(0.,0.,1.));
#10904=DIRECTION('ref_axis',(1.,0.,0.));
#10905=DIRECTION('center_axis',(0.,0.,-1.));
#10906=DIRECTION('ref_axis',(1.,0.,0.));
#10907=DIRECTION('',(0.,0.,-1.));
#10908=DIRECTION('center_axis',(0.,0.,-1.));
#10909=DIRECTION('ref_axis',(1.,0.,0.));
#10910=DIRECTION('center_axis',(0.,0.,1.));
#10911=DIRECTION('ref_axis',(1.,0.,0.));
#10912=DIRECTION('center_axis',(0.,0.,1.));
#10913=DIRECTION('ref_axis',(1.,0.,0.));
#10914=DIRECTION('',(0.,0.,-1.));
#10915=DIRECTION('center_axis',(0.,0.,1.));
#10916=DIRECTION('ref_axis',(1.,0.,0.));
#10917=DIRECTION('center_axis',(0.,0.,1.));
#10918=DIRECTION('ref_axis',(1.,0.,0.));
#10919=DIRECTION('center_axis',(0.,0.,1.));
#10920=DIRECTION('ref_axis',(1.,0.,0.));
#10921=DIRECTION('axis',(0.,0.,1.));
#10922=DIRECTION('refdir',(1.,0.,0.));
#10923=DIRECTION('center_axis',(1.,0.,0.));
#10924=DIRECTION('ref_axis',(0.,0.,-1.));
#10925=DIRECTION('',(0.,0.,1.));
#10926=DIRECTION('center_axis',(1.,0.,0.));
#10927=DIRECTION('ref_axis',(0.,0.,-1.));
#10928=DIRECTION('center_axis',(1.,0.,0.));
#10929=DIRECTION('ref_axis',(0.,0.,-1.));
#10930=DIRECTION('center_axis',(1.,0.,0.));
#10931=DIRECTION('ref_axis',(0.,0.,-1.));
#10932=DIRECTION('',(1.,0.,0.));
#10933=DIRECTION('center_axis',(1.,0.,0.));
#10934=DIRECTION('ref_axis',(0.,0.,-1.));
#10935=DIRECTION('',(0.,0.,-1.));
#10936=DIRECTION('center_axis',(0.,0.,1.));
#10937=DIRECTION('ref_axis',(1.,0.,0.));
#10938=DIRECTION('center_axis',(0.,0.,-1.));
#10939=DIRECTION('ref_axis',(1.,0.,0.));
#10940=DIRECTION('',(0.,0.,-1.));
#10941=DIRECTION('center_axis',(0.,0.,-1.));
#10942=DIRECTION('ref_axis',(1.,0.,0.));
#10943=DIRECTION('center_axis',(0.,0.,1.));
#10944=DIRECTION('ref_axis',(1.,0.,0.));
#10945=DIRECTION('center_axis',(0.,0.,1.));
#10946=DIRECTION('ref_axis',(1.,0.,0.));
#10947=DIRECTION('',(0.,0.,-1.));
#10948=DIRECTION('center_axis',(0.,0.,1.));
#10949=DIRECTION('ref_axis',(1.,0.,0.));
#10950=DIRECTION('center_axis',(0.,0.,1.));
#10951=DIRECTION('ref_axis',(1.,0.,0.));
#10952=DIRECTION('center_axis',(0.,0.,1.));
#10953=DIRECTION('ref_axis',(1.,0.,0.));
#10954=DIRECTION('axis',(0.,0.,1.));
#10955=DIRECTION('refdir',(1.,0.,0.));
#10956=DIRECTION('center_axis',(0.,0.,1.));
#10957=DIRECTION('ref_axis',(1.,0.,0.));
#10958=DIRECTION('center_axis',(0.,0.,1.));
#10959=DIRECTION('ref_axis',(1.,0.,0.));
#10960=DIRECTION('',(0.,0.,1.));
#10961=DIRECTION('center_axis',(0.,0.,-1.));
#10962=DIRECTION('ref_axis',(1.,0.,0.));
#10963=DIRECTION('center_axis',(0.,0.,1.));
#10964=DIRECTION('ref_axis',(1.,0.,0.));
#10965=DIRECTION('center_axis',(0.,0.,1.));
#10966=DIRECTION('ref_axis',(1.,0.,0.));
#10967=DIRECTION('center_axis',(0.,0.,1.));
#10968=DIRECTION('ref_axis',(1.,0.,0.));
#10969=DIRECTION('center_axis',(0.,0.,1.));
#10970=DIRECTION('ref_axis',(1.,0.,0.));
#10971=DIRECTION('center_axis',(0.,0.,1.));
#10972=DIRECTION('ref_axis',(1.,0.,0.));
#10973=DIRECTION('center_axis',(0.,0.,1.));
#10974=DIRECTION('ref_axis',(1.,0.,0.));
#10975=DIRECTION('center_axis',(0.,0.,-1.));
#10976=DIRECTION('ref_axis',(1.,0.,0.));
#10977=DIRECTION('center_axis',(0.,0.,1.));
#10978=DIRECTION('ref_axis',(1.,0.,0.));
#10979=DIRECTION('',(0.,0.,-1.));
#10980=DIRECTION('center_axis',(0.,0.,1.));
#10981=DIRECTION('ref_axis',(1.,0.,0.));
#10982=DIRECTION('',(0.,0.,-1.));
#10983=DIRECTION('center_axis',(0.,0.,1.));
#10984=DIRECTION('ref_axis',(1.,0.,0.));
#10985=DIRECTION('center_axis',(0.,0.,1.));
#10986=DIRECTION('ref_axis',(1.,0.,0.));
#10987=DIRECTION('center_axis',(0.,0.,1.));
#10988=DIRECTION('ref_axis',(1.,0.,0.));
#10989=DIRECTION('',(0.,0.,-1.));
#10990=DIRECTION('center_axis',(0.,0.,1.));
#10991=DIRECTION('ref_axis',(1.,0.,0.));
#10992=DIRECTION('center_axis',(0.,0.,1.));
#10993=DIRECTION('ref_axis',(1.,0.,0.));
#10994=DIRECTION('axis',(0.,0.,1.));
#10995=DIRECTION('refdir',(1.,0.,0.));
#10996=DIRECTION('center_axis',(0.,0.,1.));
#10997=DIRECTION('ref_axis',(1.,0.,0.));
#10998=DIRECTION('center_axis',(0.,0.,-1.));
#10999=DIRECTION('ref_axis',(1.,0.,0.));
#11000=DIRECTION('',(0.,0.,-1.));
#11001=DIRECTION('center_axis',(0.,0.,-1.));
#11002=DIRECTION('ref_axis',(1.,0.,0.));
#11003=DIRECTION('center_axis',(0.,0.,1.));
#11004=DIRECTION('ref_axis',(1.,0.,0.));
#11005=DIRECTION('center_axis',(0.,0.,1.));
#11006=DIRECTION('ref_axis',(1.,0.,0.));
#11007=DIRECTION('',(0.,0.,-1.));
#11008=DIRECTION('center_axis',(0.,0.,1.));
#11009=DIRECTION('ref_axis',(1.,0.,0.));
#11010=DIRECTION('center_axis',(0.,0.,1.));
#11011=DIRECTION('ref_axis',(1.,0.,0.));
#11012=DIRECTION('center_axis',(0.,0.,1.));
#11013=DIRECTION('ref_axis',(1.,0.,0.));
#11014=DIRECTION('axis',(0.,0.,1.));
#11015=DIRECTION('refdir',(1.,0.,0.));
#11016=DIRECTION('center_axis',(0.,0.,1.));
#11017=DIRECTION('ref_axis',(1.,0.,0.));
#11018=DIRECTION('center_axis',(0.,0.,-1.));
#11019=DIRECTION('ref_axis',(1.,0.,0.));
#11020=DIRECTION('',(0.,0.,-1.));
#11021=DIRECTION('center_axis',(0.,0.,-1.));
#11022=DIRECTION('ref_axis',(1.,0.,0.));
#11023=DIRECTION('center_axis',(0.,0.,1.));
#11024=DIRECTION('ref_axis',(1.,0.,0.));
#11025=DIRECTION('center_axis',(0.,0.,1.));
#11026=DIRECTION('ref_axis',(1.,0.,0.));
#11027=DIRECTION('',(0.,0.,-1.));
#11028=DIRECTION('center_axis',(0.,0.,1.));
#11029=DIRECTION('ref_axis',(1.,0.,0.));
#11030=DIRECTION('center_axis',(0.,0.,1.));
#11031=DIRECTION('ref_axis',(1.,0.,0.));
#11032=DIRECTION('center_axis',(0.,0.,1.));
#11033=DIRECTION('ref_axis',(1.,0.,0.));
#11034=DIRECTION('axis',(0.,0.,1.));
#11035=DIRECTION('refdir',(1.,0.,0.));
#11036=DIRECTION('center_axis',(0.,0.,1.));
#11037=DIRECTION('ref_axis',(1.,0.,0.));
#11038=DIRECTION('center_axis',(0.,0.,-1.));
#11039=DIRECTION('ref_axis',(1.,0.,0.));
#11040=DIRECTION('',(0.,0.,-1.));
#11041=DIRECTION('center_axis',(0.,0.,-1.));
#11042=DIRECTION('ref_axis',(1.,0.,0.));
#11043=DIRECTION('center_axis',(0.,0.,1.));
#11044=DIRECTION('ref_axis',(1.,0.,0.));
#11045=DIRECTION('center_axis',(0.,0.,1.));
#11046=DIRECTION('ref_axis',(1.,0.,0.));
#11047=DIRECTION('',(0.,0.,-1.));
#11048=DIRECTION('center_axis',(0.,0.,1.));
#11049=DIRECTION('ref_axis',(1.,0.,0.));
#11050=DIRECTION('center_axis',(0.,0.,1.));
#11051=DIRECTION('ref_axis',(1.,0.,0.));
#11052=DIRECTION('center_axis',(0.,0.,1.));
#11053=DIRECTION('ref_axis',(1.,0.,0.));
#11054=DIRECTION('axis',(0.,0.,1.));
#11055=DIRECTION('refdir',(1.,0.,0.));
#11056=DIRECTION('center_axis',(0.,1.,0.));
#11057=DIRECTION('ref_axis',(1.,0.,0.));
#11058=DIRECTION('center_axis',(0.,1.,0.));
#11059=DIRECTION('ref_axis',(1.,0.,0.));
#11060=DIRECTION('center_axis',(0.866025403784439,0.,-0.5));
#11061=DIRECTION('ref_axis',(0.5,0.,0.866025403784439));
#11062=DIRECTION('',(0.5,0.,0.866025403784439));
#11063=DIRECTION('',(0.,-1.,0.));
#11064=DIRECTION('',(0.5,0.,0.866025403784439));
#11065=DIRECTION('',(0.,-1.,0.));
#11066=DIRECTION('center_axis',(1.20185167898973E-16,0.,-1.));
#11067=DIRECTION('ref_axis',(1.,0.,1.20185167898973E-16));
#11068=DIRECTION('',(1.,0.,1.20185167898973E-16));
#11069=DIRECTION('',(0.,-1.,0.));
#11070=DIRECTION('',(1.,0.,1.20185167898973E-16));
#11071=DIRECTION('center_axis',(-0.866025403784439,0.,-0.5));
#11072=DIRECTION('ref_axis',(0.5,0.,-0.866025403784439));
#11073=DIRECTION('',(0.5,0.,-0.866025403784439));
#11074=DIRECTION('',(0.,-1.,0.));
#11075=DIRECTION('',(0.5,0.,-0.866025403784439));
#11076=DIRECTION('center_axis',(-0.866025403784439,0.,0.5));
#11077=DIRECTION('ref_axis',(-0.5,0.,-0.866025403784439));
#11078=DIRECTION('',(-0.5,0.,-0.866025403784439));
#11079=DIRECTION('',(0.,-1.,0.));
#11080=DIRECTION('',(-0.5,0.,-0.866025403784439));
#11081=DIRECTION('center_axis',(-2.40370335797945E-16,0.,1.));
#11082=DIRECTION('ref_axis',(-1.,0.,-2.40370335797945E-16));
#11083=DIRECTION('',(-1.,0.,-2.40370335797945E-16));
#11084=DIRECTION('',(0.,-1.,0.));
#11085=DIRECTION('',(-1.,0.,-2.40370335797945E-16));
#11086=DIRECTION('center_axis',(0.866025403784439,0.,0.5));
#11087=DIRECTION('ref_axis',(-0.5,0.,0.866025403784439));
#11088=DIRECTION('',(-0.5,0.,0.866025403784439));
#11089=DIRECTION('',(-0.5,0.,0.866025403784439));
#11090=DIRECTION('center_axis',(0.,-1.,0.));
#11091=DIRECTION('ref_axis',(0.,0.,-1.));
#11092=DIRECTION('center_axis',(0.,1.,0.));
#11093=DIRECTION('ref_axis',(0.,0.,1.));
#11094=DIRECTION('center_axis',(0.,-1.,0.));
#11095=DIRECTION('ref_axis',(1.,0.,0.));
#11096=DIRECTION('center_axis',(0.,-1.,0.));
#11097=DIRECTION('ref_axis',(1.,0.,0.));
#11098=DIRECTION('center_axis',(0.,-1.,0.));
#11099=DIRECTION('ref_axis',(1.,0.,0.));
#11100=DIRECTION('',(0.707106781186548,0.707106781186547,8.65956056235494E-17));
#11101=DIRECTION('center_axis',(0.,-1.,0.));
#11102=DIRECTION('ref_axis',(1.,0.,0.));
#11103=DIRECTION('',(0.,1.,0.));
#11104=DIRECTION('axis',(0.,0.,1.));
#11105=DIRECTION('refdir',(1.,0.,0.));
#11106=DIRECTION('axis',(0.,0.,1.));
#11107=DIRECTION('refdir',(1.,0.,0.));
#11108=DIRECTION('center_axis',(0.,0.,1.));
#11109=DIRECTION('ref_axis',(1.,0.,0.));
#11110=DIRECTION('center_axis',(0.,0.,1.));
#11111=DIRECTION('ref_axis',(1.,0.,0.));
#11112=DIRECTION('',(0.,0.,1.));
#11113=DIRECTION('center_axis',(0.,0.,-1.));
#11114=DIRECTION('ref_axis',(1.,0.,0.));
#11115=DIRECTION('center_axis',(0.,0.,1.));
#11116=DIRECTION('ref_axis',(1.,0.,0.));
#11117=DIRECTION('',(0.,1.,0.));
#11118=DIRECTION('',(-1.,0.,0.));
#11119=DIRECTION('',(0.,1.,0.));
#11120=DIRECTION('',(1.,0.,0.));
#11121=DIRECTION('center_axis',(0.,0.,1.));
#11122=DIRECTION('ref_axis',(1.,0.,0.));
#11123=DIRECTION('',(0.,-1.,0.));
#11124=DIRECTION('',(1.,0.,0.));
#11125=DIRECTION('',(0.,-1.,0.));
#11126=DIRECTION('',(-1.,0.,0.));
#11127=DIRECTION('center_axis',(1.,0.,0.));
#11128=DIRECTION('ref_axis',(0.,1.,0.));
#11129=DIRECTION('',(0.,0.,1.));
#11130=DIRECTION('',(0.,1.,0.));
#11131=DIRECTION('',(0.,0.,1.));
#11132=DIRECTION('center_axis',(-1.,0.,0.));
#11133=DIRECTION('ref_axis',(0.,-1.,0.));
#11134=DIRECTION('',(0.,0.,1.));
#11135=DIRECTION('',(0.,-1.,0.));
#11136=DIRECTION('',(0.,0.,1.));
#11137=DIRECTION('center_axis',(0.,0.,1.));
#11138=DIRECTION('ref_axis',(1.,0.,0.));
#11139=DIRECTION('',(1.,0.,0.));
#11140=DIRECTION('',(-1.,0.,0.));
#11141=DIRECTION('center_axis',(0.,0.,1.));
#11142=DIRECTION('ref_axis',(1.,0.,0.));
#11143=DIRECTION('',(0.,-1.,0.));
#11144=DIRECTION('',(-1.,0.,0.));
#11145=DIRECTION('',(0.,-1.,0.));
#11146=DIRECTION('',(1.,0.,0.));
#11147=DIRECTION('center_axis',(0.,0.,1.));
#11148=DIRECTION('ref_axis',(1.,0.,0.));
#11149=DIRECTION('',(0.,1.,0.));
#11150=DIRECTION('',(1.,0.,0.));
#11151=DIRECTION('',(0.,1.,0.));
#11152=DIRECTION('',(-1.,0.,0.));
#11153=DIRECTION('center_axis',(1.,0.,0.));
#11154=DIRECTION('ref_axis',(0.,1.,0.));
#11155=DIRECTION('',(0.,1.,0.));
#11156=DIRECTION('',(0.,0.,1.));
#11157=DIRECTION('',(0.,0.,1.));
#11158=DIRECTION('center_axis',(-1.,0.,0.));
#11159=DIRECTION('ref_axis',(0.,-1.,0.));
#11160=DIRECTION('',(0.,-1.,0.));
#11161=DIRECTION('',(0.,0.,1.));
#11162=DIRECTION('',(0.,0.,1.));
#11163=DIRECTION('center_axis',(0.,0.,1.));
#11164=DIRECTION('ref_axis',(1.,0.,0.));
#11165=DIRECTION('',(-1.,0.,0.));
#11166=DIRECTION('',(1.,0.,0.));
#11167=DIRECTION('center_axis',(0.,1.,0.));
#11168=DIRECTION('ref_axis',(-1.,0.,0.));
#11169=DIRECTION('',(0.,0.,1.));
#11170=DIRECTION('',(0.,0.,1.));
#11171=DIRECTION('center_axis',(1.,0.,0.));
#11172=DIRECTION('ref_axis',(0.,1.,0.));
#11173=DIRECTION('',(0.,0.,1.));
#11174=DIRECTION('center_axis',(0.,-1.,0.));
#11175=DIRECTION('ref_axis',(1.,0.,0.));
#11176=DIRECTION('',(0.,0.,1.));
#11177=DIRECTION('center_axis',(-1.,0.,0.));
#11178=DIRECTION('ref_axis',(0.,-1.,0.));
#11179=DIRECTION('',(0.,0.,1.));
#11180=DIRECTION('',(1.,0.,0.));
#11181=DIRECTION('axis',(0.,0.,1.));
#11182=DIRECTION('refdir',(1.,0.,0.));
#11183=DIRECTION('axis',(0.,0.,1.));
#11184=DIRECTION('refdir',(1.,0.,0.));
#11185=DIRECTION('center_axis',(0.,0.,1.));
#11186=DIRECTION('ref_axis',(1.,0.,0.));
#11187=DIRECTION('center_axis',(0.,0.,1.));
#11188=DIRECTION('ref_axis',(1.,0.,0.));
#11189=DIRECTION('',(0.,0.,1.));
#11190=DIRECTION('center_axis',(0.,0.,-1.));
#11191=DIRECTION('ref_axis',(1.,0.,0.));
#11192=DIRECTION('center_axis',(0.,0.,1.));
#11193=DIRECTION('ref_axis',(1.,0.,0.));
#11194=DIRECTION('center_axis',(0.,0.,1.));
#11195=DIRECTION('ref_axis',(1.,0.,0.));
#11196=DIRECTION('',(0.,0.,1.));
#11197=DIRECTION('center_axis',(0.,0.,-1.));
#11198=DIRECTION('ref_axis',(1.,0.,0.));
#11199=DIRECTION('center_axis',(0.,0.,1.));
#11200=DIRECTION('ref_axis',(1.,0.,0.));
#11201=DIRECTION('',(0.,0.,-1.));
#11202=DIRECTION('center_axis',(0.,0.,1.));
#11203=DIRECTION('ref_axis',(1.,0.,0.));
#11204=DIRECTION('',(0.,0.,1.));
#11205=DIRECTION('center_axis',(0.,0.,1.));
#11206=DIRECTION('ref_axis',(1.,0.,0.));
#11207=DIRECTION('center_axis',(-0.4,0.916515138991168,0.));
#11208=DIRECTION('ref_axis',(-0.916515138991168,-0.4,0.));
#11209=DIRECTION('',(0.916515138991168,0.4,0.));
#11210=DIRECTION('',(0.,0.,-1.));
#11211=DIRECTION('',(-0.916515138991168,-0.4,0.));
#11212=DIRECTION('center_axis',(0.,0.,1.));
#11213=DIRECTION('ref_axis',(1.,0.,0.));
#11214=DIRECTION('',(-0.916515138991168,-0.4,0.));
#11215=DIRECTION('center_axis',(0.,0.,1.));
#11216=DIRECTION('ref_axis',(1.,0.,0.));
#11217=DIRECTION('center_axis',(0.4,-0.916515138991168,0.));
#11218=DIRECTION('ref_axis',(0.916515138991168,0.4,0.));
#11219=DIRECTION('',(0.916515138991168,0.4,0.));
#11220=DIRECTION('',(0.,0.,1.));
#11221=DIRECTION('center_axis',(0.,0.,1.));
#11222=DIRECTION('ref_axis',(-0.916515138991168,-0.4,0.));
#11223=DIRECTION('center_axis',(0.,0.,1.));
#11224=DIRECTION('ref_axis',(1.,0.,0.));
#11225=DIRECTION('center_axis',(0.,0.,1.));
#11226=DIRECTION('ref_axis',(1.,0.,0.));
#11227=DIRECTION('axis',(0.,0.,1.));
#11228=DIRECTION('refdir',(1.,0.,0.));
#11229=DIRECTION('center_axis',(0.,0.,1.));
#11230=DIRECTION('ref_axis',(1.,0.,0.));
#11231=DIRECTION('center_axis',(0.,0.,-1.));
#11232=DIRECTION('ref_axis',(1.,0.,0.));
#11233=DIRECTION('',(0.,0.,-1.));
#11234=DIRECTION('center_axis',(0.,0.,-1.));
#11235=DIRECTION('ref_axis',(1.,0.,0.));
#11236=DIRECTION('center_axis',(0.,0.,1.));
#11237=DIRECTION('ref_axis',(1.,0.,0.));
#11238=DIRECTION('center_axis',(0.,0.,1.));
#11239=DIRECTION('ref_axis',(1.,0.,0.));
#11240=DIRECTION('',(0.,0.,-1.));
#11241=DIRECTION('center_axis',(0.,0.,1.));
#11242=DIRECTION('ref_axis',(1.,0.,0.));
#11243=DIRECTION('center_axis',(0.,0.,1.));
#11244=DIRECTION('ref_axis',(1.,0.,0.));
#11245=DIRECTION('center_axis',(0.,0.,1.));
#11246=DIRECTION('ref_axis',(1.,0.,0.));
#11247=DIRECTION('axis',(0.,0.,1.));
#11248=DIRECTION('refdir',(1.,0.,0.));
#11249=DIRECTION('center_axis',(0.,0.,1.));
#11250=DIRECTION('ref_axis',(1.,0.,0.));
#11251=DIRECTION('center_axis',(0.,0.,-1.));
#11252=DIRECTION('ref_axis',(1.,0.,0.));
#11253=DIRECTION('',(0.,0.,-1.));
#11254=DIRECTION('center_axis',(0.,0.,-1.));
#11255=DIRECTION('ref_axis',(1.,0.,0.));
#11256=DIRECTION('center_axis',(0.,0.,1.));
#11257=DIRECTION('ref_axis',(1.,0.,0.));
#11258=DIRECTION('center_axis',(0.,0.,1.));
#11259=DIRECTION('ref_axis',(1.,0.,0.));
#11260=DIRECTION('',(0.,0.,-1.));
#11261=DIRECTION('center_axis',(0.,0.,1.));
#11262=DIRECTION('ref_axis',(1.,0.,0.));
#11263=DIRECTION('center_axis',(0.,0.,1.));
#11264=DIRECTION('ref_axis',(1.,0.,0.));
#11265=DIRECTION('center_axis',(0.,0.,1.));
#11266=DIRECTION('ref_axis',(1.,0.,0.));
#11267=DIRECTION('',(0.,0.,1.));
#11268=DIRECTION('',(1.,0.,0.));
#11269=DIRECTION('',(0.,0.,1.));
#11270=DIRECTION('',(1.,0.,0.));
#11271=DIRECTION('',(0.,0.,1.));
#11272=DIRECTION('',(1.,0.,0.));
#11273=DIRECTION('axis',(0.,0.,1.));
#11274=DIRECTION('refdir',(1.,0.,0.));
#11275=DIRECTION('axis',(0.,0.,1.));
#11276=DIRECTION('refdir',(1.,0.,0.));
#11277=DIRECTION('center_axis',(0.,0.,1.));
#11278=DIRECTION('ref_axis',(1.,0.,0.));
#11279=DIRECTION('center_axis',(0.,0.,1.));
#11280=DIRECTION('ref_axis',(1.,0.,0.));
#11281=DIRECTION('',(0.,0.,1.));
#11282=DIRECTION('center_axis',(0.,0.,-1.));
#11283=DIRECTION('ref_axis',(1.,0.,0.));
#11284=DIRECTION('center_axis',(0.,0.,1.));
#11285=DIRECTION('ref_axis',(1.,0.,0.));
#11286=DIRECTION('center_axis',(0.,0.,1.));
#11287=DIRECTION('ref_axis',(1.,0.,0.));
#11288=DIRECTION('',(0.,0.,1.));
#11289=DIRECTION('center_axis',(0.,0.,-1.));
#11290=DIRECTION('ref_axis',(1.,0.,0.));
#11291=DIRECTION('center_axis',(0.,0.,1.));
#11292=DIRECTION('ref_axis',(1.,0.,0.));
#11293=DIRECTION('center_axis',(0.,0.,1.));
#11294=DIRECTION('ref_axis',(1.,0.,0.));
#11295=DIRECTION('',(0.,0.,1.));
#11296=DIRECTION('center_axis',(0.,0.,-1.));
#11297=DIRECTION('ref_axis',(1.,0.,0.));
#11298=DIRECTION('center_axis',(0.,0.,1.));
#11299=DIRECTION('ref_axis',(1.,0.,0.));
#11300=DIRECTION('center_axis',(0.,0.,1.));
#11301=DIRECTION('ref_axis',(1.,0.,0.));
#11302=DIRECTION('',(0.,0.,1.));
#11303=DIRECTION('center_axis',(0.,0.,-1.));
#11304=DIRECTION('ref_axis',(1.,0.,0.));
#11305=DIRECTION('center_axis',(0.,0.,1.));
#11306=DIRECTION('ref_axis',(1.,0.,0.));
#11307=DIRECTION('center_axis',(0.,0.,1.));
#11308=DIRECTION('ref_axis',(1.,0.,0.));
#11309=DIRECTION('',(0.,0.,1.));
#11310=DIRECTION('center_axis',(0.,0.,-1.));
#11311=DIRECTION('ref_axis',(1.,0.,0.));
#11312=DIRECTION('center_axis',(0.,1.,0.));
#11313=DIRECTION('ref_axis',(-1.,0.,0.));
#11314=DIRECTION('',(-1.,0.,0.));
#11315=DIRECTION('',(0.,0.,1.));
#11316=DIRECTION('',(-1.,0.,0.));
#11317=DIRECTION('',(0.,0.,1.));
#11318=DIRECTION('center_axis',(1.,0.,0.));
#11319=DIRECTION('ref_axis',(0.,1.,0.));
#11320=DIRECTION('',(0.,1.,0.));
#11321=DIRECTION('',(0.,1.,0.));
#11322=DIRECTION('',(0.,0.,1.));
#11323=DIRECTION('center_axis',(0.,-1.,0.));
#11324=DIRECTION('ref_axis',(1.,0.,0.));
#11325=DIRECTION('',(1.,0.,0.));
#11326=DIRECTION('',(1.,0.,0.));
#11327=DIRECTION('',(0.,0.,1.));
#11328=DIRECTION('center_axis',(-1.,0.,0.));
#11329=DIRECTION('ref_axis',(0.,-1.,0.));
#11330=DIRECTION('',(0.,-1.,0.));
#11331=DIRECTION('',(0.,-1.,0.));
#11332=DIRECTION('center_axis',(0.,0.,1.));
#11333=DIRECTION('ref_axis',(1.,0.,0.));
#11334=DIRECTION('center_axis',(0.,0.,1.));
#11335=DIRECTION('ref_axis',(1.,0.,0.));
#11336=DIRECTION('axis',(0.,0.,1.));
#11337=DIRECTION('refdir',(1.,0.,0.));
#11338=DIRECTION('center_axis',(0.,0.,1.));
#11339=DIRECTION('ref_axis',(1.,0.,0.));
#11340=DIRECTION('center_axis',(0.,0.,1.));
#11341=DIRECTION('ref_axis',(1.,0.,0.));
#11342=DIRECTION('',(0.,0.,1.));
#11343=DIRECTION('center_axis',(0.,0.,-1.));
#11344=DIRECTION('ref_axis',(1.,0.,0.));
#11345=DIRECTION('center_axis',(0.,0.,1.));
#11346=DIRECTION('ref_axis',(1.,0.,0.));
#11347=DIRECTION('center_axis',(0.,0.,1.));
#11348=DIRECTION('ref_axis',(1.,0.,0.));
#11349=DIRECTION('center_axis',(0.,0.,1.));
#11350=DIRECTION('ref_axis',(1.,0.,0.));
#11351=DIRECTION('center_axis',(0.,0.,1.));
#11352=DIRECTION('ref_axis',(1.,0.,0.));
#11353=DIRECTION('center_axis',(0.,0.,1.));
#11354=DIRECTION('ref_axis',(1.,0.,0.));
#11355=DIRECTION('center_axis',(0.,0.,1.));
#11356=DIRECTION('ref_axis',(1.,0.,0.));
#11357=DIRECTION('center_axis',(0.,0.,-1.));
#11358=DIRECTION('ref_axis',(1.,0.,0.));
#11359=DIRECTION('center_axis',(0.,0.,1.));
#11360=DIRECTION('ref_axis',(1.,0.,0.));
#11361=DIRECTION('',(0.,0.,-1.));
#11362=DIRECTION('center_axis',(0.,0.,1.));
#11363=DIRECTION('ref_axis',(1.,0.,0.));
#11364=DIRECTION('',(0.,0.,-1.));
#11365=DIRECTION('center_axis',(0.,0.,1.));
#11366=DIRECTION('ref_axis',(1.,0.,0.));
#11367=DIRECTION('center_axis',(0.,0.,1.));
#11368=DIRECTION('ref_axis',(1.,0.,0.));
#11369=DIRECTION('center_axis',(0.,0.,1.));
#11370=DIRECTION('ref_axis',(1.,0.,0.));
#11371=DIRECTION('',(0.,0.,-1.));
#11372=DIRECTION('center_axis',(0.,0.,1.));
#11373=DIRECTION('ref_axis',(1.,0.,0.));
#11374=DIRECTION('center_axis',(0.,0.,1.));
#11375=DIRECTION('ref_axis',(1.,0.,0.));
#11376=DIRECTION('axis',(0.,0.,1.));
#11377=DIRECTION('refdir',(1.,0.,0.));
#11378=DIRECTION('center_axis',(0.,0.,1.));
#11379=DIRECTION('ref_axis',(1.,0.,0.));
#11380=DIRECTION('center_axis',(0.,0.,-1.));
#11381=DIRECTION('ref_axis',(1.,0.,0.));
#11382=DIRECTION('',(0.,0.,-1.));
#11383=DIRECTION('center_axis',(0.,0.,-1.));
#11384=DIRECTION('ref_axis',(1.,0.,0.));
#11385=DIRECTION('center_axis',(0.,0.,1.));
#11386=DIRECTION('ref_axis',(1.,0.,0.));
#11387=DIRECTION('center_axis',(0.,0.,1.));
#11388=DIRECTION('ref_axis',(1.,0.,0.));
#11389=DIRECTION('',(0.,0.,-1.));
#11390=DIRECTION('center_axis',(0.,0.,1.));
#11391=DIRECTION('ref_axis',(1.,0.,0.));
#11392=DIRECTION('center_axis',(0.,0.,1.));
#11393=DIRECTION('ref_axis',(1.,0.,0.));
#11394=DIRECTION('center_axis',(0.,0.,1.));
#11395=DIRECTION('ref_axis',(1.,0.,0.));
#11396=DIRECTION('axis',(0.,0.,1.));
#11397=DIRECTION('refdir',(1.,0.,0.));
#11398=DIRECTION('center_axis',(0.,0.,1.));
#11399=DIRECTION('ref_axis',(1.,0.,0.));
#11400=DIRECTION('center_axis',(0.,0.,-1.));
#11401=DIRECTION('ref_axis',(1.,0.,0.));
#11402=DIRECTION('',(0.,0.,-1.));
#11403=DIRECTION('center_axis',(0.,0.,-1.));
#11404=DIRECTION('ref_axis',(1.,0.,0.));
#11405=DIRECTION('center_axis',(0.,0.,1.));
#11406=DIRECTION('ref_axis',(1.,0.,0.));
#11407=DIRECTION('center_axis',(0.,0.,1.));
#11408=DIRECTION('ref_axis',(1.,0.,0.));
#11409=DIRECTION('',(0.,0.,-1.));
#11410=DIRECTION('center_axis',(0.,0.,1.));
#11411=DIRECTION('ref_axis',(1.,0.,0.));
#11412=DIRECTION('center_axis',(0.,0.,1.));
#11413=DIRECTION('ref_axis',(1.,0.,0.));
#11414=DIRECTION('center_axis',(0.,0.,1.));
#11415=DIRECTION('ref_axis',(1.,0.,0.));
#11416=DIRECTION('axis',(0.,0.,1.));
#11417=DIRECTION('refdir',(1.,0.,0.));
#11418=DIRECTION('center_axis',(0.,0.,1.));
#11419=DIRECTION('ref_axis',(1.,0.,0.));
#11420=DIRECTION('center_axis',(0.,0.,-1.));
#11421=DIRECTION('ref_axis',(1.,0.,0.));
#11422=DIRECTION('',(0.,0.,-1.));
#11423=DIRECTION('center_axis',(0.,0.,-1.));
#11424=DIRECTION('ref_axis',(1.,0.,0.));
#11425=DIRECTION('center_axis',(0.,0.,1.));
#11426=DIRECTION('ref_axis',(1.,0.,0.));
#11427=DIRECTION('center_axis',(0.,0.,1.));
#11428=DIRECTION('ref_axis',(1.,0.,0.));
#11429=DIRECTION('',(0.,0.,-1.));
#11430=DIRECTION('center_axis',(0.,0.,1.));
#11431=DIRECTION('ref_axis',(1.,0.,0.));
#11432=DIRECTION('center_axis',(0.,0.,1.));
#11433=DIRECTION('ref_axis',(1.,0.,0.));
#11434=DIRECTION('center_axis',(0.,0.,1.));
#11435=DIRECTION('ref_axis',(1.,0.,0.));
#11436=DIRECTION('axis',(0.,0.,1.));
#11437=DIRECTION('refdir',(1.,0.,0.));
#11438=DIRECTION('axis',(0.,0.,1.));
#11439=DIRECTION('refdir',(1.,0.,0.));
#11440=DIRECTION('center_axis',(0.,0.,1.));
#11441=DIRECTION('ref_axis',(1.,0.,0.));
#11442=DIRECTION('',(-1.,0.,0.));
#11443=DIRECTION('center_axis',(0.,0.,1.));
#11444=DIRECTION('ref_axis',(1.,0.,0.));
#11445=DIRECTION('center_axis',(0.,0.,1.));
#11446=DIRECTION('ref_axis',(1.,0.,0.));
#11447=DIRECTION('',(0.,0.,-1.));
#11448=DIRECTION('center_axis',(0.,0.,1.));
#11449=DIRECTION('ref_axis',(1.,0.,0.));
#11450=DIRECTION('',(0.,0.,1.));
#11451=DIRECTION('center_axis',(0.,0.,-1.));
#11452=DIRECTION('ref_axis',(1.,0.,0.));
#11453=DIRECTION('center_axis',(0.,0.,1.));
#11454=DIRECTION('ref_axis',(1.,0.,0.));
#11455=DIRECTION('',(0.,0.,1.));
#11456=DIRECTION('center_axis',(0.,0.,1.));
#11457=DIRECTION('ref_axis',(1.,0.,0.));
#11458=DIRECTION('',(1.,0.,0.));
#11459=DIRECTION('center_axis',(0.,0.,1.));
#11460=DIRECTION('ref_axis',(1.,0.,0.));
#11461=DIRECTION('center_axis',(0.,0.,1.));
#11462=DIRECTION('ref_axis',(1.,0.,0.));
#11463=DIRECTION('',(0.,0.,-1.));
#11464=DIRECTION('center_axis',(0.,0.,1.));
#11465=DIRECTION('ref_axis',(1.,0.,0.));
#11466=DIRECTION('',(0.,0.,1.));
#11467=DIRECTION('center_axis',(0.,0.,-1.));
#11468=DIRECTION('ref_axis',(1.,0.,0.));
#11469=DIRECTION('center_axis',(0.,0.,1.));
#11470=DIRECTION('ref_axis',(1.,0.,0.));
#11471=DIRECTION('',(0.,0.,1.));
#11472=DIRECTION('center_axis',(0.,0.,1.));
#11473=DIRECTION('ref_axis',(1.,0.,0.));
#11474=DIRECTION('',(-1.,0.,0.));
#11475=DIRECTION('center_axis',(0.,0.,1.));
#11476=DIRECTION('ref_axis',(1.,0.,0.));
#11477=DIRECTION('center_axis',(0.,0.,1.));
#11478=DIRECTION('ref_axis',(1.,0.,0.));
#11479=DIRECTION('',(0.,0.,-1.));
#11480=DIRECTION('center_axis',(0.,0.,1.));
#11481=DIRECTION('ref_axis',(1.,0.,0.));
#11482=DIRECTION('',(0.,0.,1.));
#11483=DIRECTION('center_axis',(0.,0.,-1.));
#11484=DIRECTION('ref_axis',(1.,0.,0.));
#11485=DIRECTION('center_axis',(0.,0.,1.));
#11486=DIRECTION('ref_axis',(1.,0.,0.));
#11487=DIRECTION('',(0.,0.,1.));
#11488=DIRECTION('center_axis',(0.,0.,1.));
#11489=DIRECTION('ref_axis',(1.,0.,0.));
#11490=DIRECTION('',(1.,0.,0.));
#11491=DIRECTION('center_axis',(0.,0.,1.));
#11492=DIRECTION('ref_axis',(1.,0.,0.));
#11493=DIRECTION('center_axis',(0.,0.,1.));
#11494=DIRECTION('ref_axis',(1.,0.,0.));
#11495=DIRECTION('',(0.,0.,-1.));
#11496=DIRECTION('center_axis',(0.,0.,1.));
#11497=DIRECTION('ref_axis',(1.,0.,0.));
#11498=DIRECTION('',(0.,0.,1.));
#11499=DIRECTION('center_axis',(0.,0.,-1.));
#11500=DIRECTION('ref_axis',(1.,0.,0.));
#11501=DIRECTION('center_axis',(0.,0.,1.));
#11502=DIRECTION('ref_axis',(1.,0.,0.));
#11503=DIRECTION('',(0.,0.,1.));
#11504=DIRECTION('center_axis',(0.,-1.,0.));
#11505=DIRECTION('ref_axis',(0.,0.,-1.));
#11506=DIRECTION('',(-1.,0.,0.));
#11507=DIRECTION('',(-1.,0.,0.));
#11508=DIRECTION('',(0.,0.,1.));
#11509=DIRECTION('',(1.,0.,0.));
#11510=DIRECTION('',(0.,0.,-1.));
#11511=DIRECTION('',(-1.,0.,0.));
#11512=DIRECTION('center_axis',(0.,1.,0.));
#11513=DIRECTION('ref_axis',(0.,0.,1.));
#11514=DIRECTION('',(1.,0.,0.));
#11515=DIRECTION('',(1.,0.,0.));
#11516=DIRECTION('',(0.,0.,1.));
#11517=DIRECTION('',(1.,0.,0.));
#11518=DIRECTION('',(0.,0.,-1.));
#11519=DIRECTION('',(1.,0.,0.));
#11520=DIRECTION('center_axis',(-1.,0.,0.));
#11521=DIRECTION('ref_axis',(0.,0.,1.));
#11522=DIRECTION('',(0.,-1.,0.));
#11523=DIRECTION('',(0.,0.,1.));
#11524=DIRECTION('',(0.,1.,0.));
#11525=DIRECTION('',(0.,0.,-1.));
#11526=DIRECTION('',(0.,-1.,0.));
#11527=DIRECTION('',(0.,-1.,0.));
#11528=DIRECTION('',(0.,0.,1.));
#11529=DIRECTION('',(0.,-1.,0.));
#11530=DIRECTION('',(0.,0.,-1.));
#11531=DIRECTION('',(0.,-1.,0.));
#11532=DIRECTION('center_axis',(0.,0.,-1.));
#11533=DIRECTION('ref_axis',(0.,1.,0.));
#11534=DIRECTION('',(0.,1.,0.));
#11535=DIRECTION('',(1.,0.,0.));
#11536=DIRECTION('center_axis',(0.,-1.,0.));
#11537=DIRECTION('ref_axis',(0.,0.,-1.));
#11538=DIRECTION('',(0.,0.,-1.));
#11539=DIRECTION('',(1.,0.,0.));
#11540=DIRECTION('center_axis',(0.,0.,1.));
#11541=DIRECTION('ref_axis',(0.,-1.,0.));
#11542=DIRECTION('',(0.,-1.,0.));
#11543=DIRECTION('',(1.,0.,0.));
#11544=DIRECTION('center_axis',(0.,1.,0.));
#11545=DIRECTION('ref_axis',(0.,0.,1.));
#11546=DIRECTION('',(0.,0.,1.));
#11547=DIRECTION('',(1.,0.,0.));
#11548=DIRECTION('center_axis',(0.,0.,-1.));
#11549=DIRECTION('ref_axis',(0.,1.,0.));
#11550=DIRECTION('',(0.,1.,0.));
#11551=DIRECTION('center_axis',(0.,0.,-1.));
#11552=DIRECTION('ref_axis',(0.,1.,0.));
#11553=DIRECTION('',(0.,1.,0.));
#11554=DIRECTION('',(1.,0.,0.));
#11555=DIRECTION('center_axis',(0.,-1.,0.));
#11556=DIRECTION('ref_axis',(0.,0.,-1.));
#11557=DIRECTION('',(0.,0.,-1.));
#11558=DIRECTION('',(1.,0.,0.));
#11559=DIRECTION('center_axis',(0.,0.,-1.));
#11560=DIRECTION('ref_axis',(0.,1.,0.));
#11561=DIRECTION('',(0.,1.,0.));
#11562=DIRECTION('',(1.,0.,0.));
#11563=DIRECTION('center_axis',(0.,1.,0.));
#11564=DIRECTION('ref_axis',(0.,0.,1.));
#11565=DIRECTION('',(0.,0.,1.));
#11566=DIRECTION('',(1.,0.,0.));
#11567=DIRECTION('center_axis',(0.,0.,-1.));
#11568=DIRECTION('ref_axis',(0.,1.,0.));
#11569=DIRECTION('',(0.,1.,0.));
#11570=DIRECTION('center_axis',(1.,0.,0.));
#11571=DIRECTION('ref_axis',(0.,0.,-1.));
#11572=DIRECTION('axis',(0.,0.,1.));
#11573=DIRECTION('refdir',(1.,0.,0.));
#11574=DIRECTION('center_axis',(0.,0.,1.));
#11575=DIRECTION('ref_axis',(0.,-1.,0.));
#11576=DIRECTION('',(0.,-1.,0.));
#11577=DIRECTION('',(1.,0.,0.));
#11578=DIRECTION('',(0.,-1.,0.));
#11579=DIRECTION('',(1.,0.,0.));
#11580=DIRECTION('center_axis',(0.,1.,0.));
#11581=DIRECTION('ref_axis',(0.,0.,1.));
#11582=DIRECTION('',(0.,0.,1.));
#11583=DIRECTION('',(0.,0.,1.));
#11584=DIRECTION('',(1.,0.,0.));
#11585=DIRECTION('center_axis',(0.,0.,-1.));
#11586=DIRECTION('ref_axis',(0.,1.,0.));
#11587=DIRECTION('',(0.,1.,0.));
#11588=DIRECTION('',(0.,1.,0.));
#11589=DIRECTION('',(1.,0.,0.));
#11590=DIRECTION('center_axis',(0.,-1.,0.));
#11591=DIRECTION('ref_axis',(0.,0.,-1.));
#11592=DIRECTION('',(0.,0.,-1.));
#11593=DIRECTION('',(0.,0.,-1.));
#11594=DIRECTION('',(1.,0.,0.));
#11595=DIRECTION('center_axis',(0.,0.,-1.));
#11596=DIRECTION('ref_axis',(0.,1.,0.));
#11597=DIRECTION('',(0.,1.,0.));
#11598=DIRECTION('',(0.,1.,0.));
#11599=DIRECTION('',(1.,0.,0.));
#11600=DIRECTION('center_axis',(0.,1.,0.));
#11601=DIRECTION('ref_axis',(0.,0.,1.));
#11602=DIRECTION('',(0.,0.,1.));
#11603=DIRECTION('',(0.,0.,1.));
#11604=DIRECTION('',(1.,0.,0.));
#11605=DIRECTION('center_axis',(0.,0.,-1.));
#11606=DIRECTION('ref_axis',(0.,1.,0.));
#11607=DIRECTION('',(0.,1.,0.));
#11608=DIRECTION('',(0.,1.,0.));
#11609=DIRECTION('',(1.,0.,0.));
#11610=DIRECTION('center_axis',(0.,-1.,0.));
#11611=DIRECTION('ref_axis',(0.,0.,-1.));
#11612=DIRECTION('',(0.,0.,-1.));
#11613=DIRECTION('',(0.,0.,-1.));
#11614=DIRECTION('center_axis',(1.,0.,0.));
#11615=DIRECTION('ref_axis',(0.,0.,-1.));
#11616=DIRECTION('center_axis',(1.,0.,0.));
#11617=DIRECTION('ref_axis',(0.,0.,-1.));
#11618=DIRECTION('axis',(0.,0.,1.));
#11619=DIRECTION('refdir',(1.,0.,0.));
#11620=DIRECTION('center_axis',(0.,0.,-1.));
#11621=DIRECTION('ref_axis',(0.,-1.,0.));
#11622=DIRECTION('',(0.,1.,0.));
#11623=DIRECTION('',(-1.,0.,0.));
#11624=DIRECTION('',(0.,-1.,0.));
#11625=DIRECTION('',(-1.,0.,0.));
#11626=DIRECTION('center_axis',(0.,1.,0.));
#11627=DIRECTION('ref_axis',(0.,0.,-1.));
#11628=DIRECTION('',(0.,0.,1.));
#11629=DIRECTION('',(0.,0.,-1.));
#11630=DIRECTION('',(-1.,0.,0.));
#11631=DIRECTION('center_axis',(0.,0.,-1.));
#11632=DIRECTION('ref_axis',(0.,-1.,0.));
#11633=DIRECTION('',(0.,1.,0.));
#11634=DIRECTION('',(0.,-1.,0.));
#11635=DIRECTION('',(-1.,0.,0.));
#11636=DIRECTION('center_axis',(0.,-1.,0.));
#11637=DIRECTION('ref_axis',(0.,0.,1.));
#11638=DIRECTION('',(0.,0.,-1.));
#11639=DIRECTION('',(0.,0.,1.));
#11640=DIRECTION('',(-1.,0.,0.));
#11641=DIRECTION('center_axis',(0.,0.,-1.));
#11642=DIRECTION('ref_axis',(0.,-1.,0.));
#11643=DIRECTION('',(0.,1.,0.));
#11644=DIRECTION('',(0.,-1.,0.));
#11645=DIRECTION('',(-1.,0.,0.));
#11646=DIRECTION('center_axis',(0.,1.,0.));
#11647=DIRECTION('ref_axis',(0.,0.,-1.));
#11648=DIRECTION('',(0.,0.,1.));
#11649=DIRECTION('',(0.,0.,-1.));
#11650=DIRECTION('',(-1.,0.,0.));
#11651=DIRECTION('center_axis',(0.,0.,1.));
#11652=DIRECTION('ref_axis',(0.,1.,0.));
#11653=DIRECTION('',(0.,-1.,0.));
#11654=DIRECTION('',(0.,1.,0.));
#11655=DIRECTION('',(-1.,0.,0.));
#11656=DIRECTION('center_axis',(0.,-1.,0.));
#11657=DIRECTION('ref_axis',(0.,0.,1.));
#11658=DIRECTION('',(0.,0.,-1.));
#11659=DIRECTION('',(0.,0.,1.));
#11660=DIRECTION('center_axis',(1.,0.,0.));
#11661=DIRECTION('ref_axis',(0.,0.,-1.));
#11662=DIRECTION('center_axis',(-1.,0.,0.));
#11663=DIRECTION('ref_axis',(0.,0.,1.));
#11664=DIRECTION('',(0.,0.,1.));
#11665=DIRECTION('',(1.,0.,0.));
#11666=DIRECTION('',(0.,0.,1.));
#11667=DIRECTION('',(1.,0.,0.));
#11668=DIRECTION('',(0.,0.,1.));
#11669=DIRECTION('',(1.,0.,0.));
#11670=DIRECTION('axis',(0.,0.,1.));
#11671=DIRECTION('refdir',(1.,0.,0.));
#11672=DIRECTION('center_axis',(0.866025403784439,0.,-0.5));
#11673=DIRECTION('ref_axis',(0.5,0.,0.866025403784439));
#11674=DIRECTION('',(-0.5,0.,-0.866025403784439));
#11675=DIRECTION('',(0.,-1.,0.));
#11676=DIRECTION('',(0.5,0.,0.866025403784439));
#11677=DIRECTION('',(0.,-1.,0.));
#11678=DIRECTION('center_axis',(1.20185167898973E-16,0.,-1.));
#11679=DIRECTION('ref_axis',(1.,0.,1.20185167898973E-16));
#11680=DIRECTION('',(-1.,0.,-1.20185167898973E-16));
#11681=DIRECTION('',(0.,-1.,0.));
#11682=DIRECTION('',(1.,0.,1.20185167898973E-16));
#11683=DIRECTION('center_axis',(-0.866025403784439,0.,-0.5));
#11684=DIRECTION('ref_axis',(0.5,0.,-0.866025403784439));
#11685=DIRECTION('',(-0.5,0.,0.866025403784439));
#11686=DIRECTION('',(0.,-1.,0.));
#11687=DIRECTION('',(0.5,0.,-0.866025403784439));
#11688=DIRECTION('center_axis',(-0.866025403784439,0.,0.5));
#11689=DIRECTION('ref_axis',(-0.5,0.,-0.866025403784439));
#11690=DIRECTION('',(0.5,0.,0.866025403784439));
#11691=DIRECTION('',(0.,-1.,0.));
#11692=DIRECTION('',(-0.5,0.,-0.866025403784439));
#11693=DIRECTION('center_axis',(-2.40370335797945E-16,0.,1.));
#11694=DIRECTION('ref_axis',(-1.,0.,-2.40370335797945E-16));
#11695=DIRECTION('',(1.,0.,2.40370335797945E-16));
#11696=DIRECTION('',(0.,-1.,0.));
#11697=DIRECTION('',(-1.,0.,-2.40370335797945E-16));
#11698=DIRECTION('center_axis',(0.866025403784439,0.,0.5));
#11699=DIRECTION('ref_axis',(-0.5,0.,0.866025403784439));
#11700=DIRECTION('',(0.5,0.,-0.866025403784439));
#11701=DIRECTION('',(-0.5,0.,0.866025403784439));
#11702=DIRECTION('center_axis',(0.,1.,0.));
#11703=DIRECTION('ref_axis',(1.,0.,0.));
#11704=DIRECTION('center_axis',(0.,-1.,0.));
#11705=DIRECTION('ref_axis',(0.,0.,-1.));
#11706=DIRECTION('center_axis',(0.,1.,0.));
#11707=DIRECTION('ref_axis',(1.,0.,0.));
#11708=DIRECTION('center_axis',(0.,1.,0.));
#11709=DIRECTION('ref_axis',(1.,0.,0.));
#11710=DIRECTION('center_axis',(0.,1.,0.));
#11711=DIRECTION('ref_axis',(0.,0.,1.));
#11712=DIRECTION('center_axis',(0.,-1.,0.));
#11713=DIRECTION('ref_axis',(1.,0.,0.));
#11714=DIRECTION('center_axis',(0.,-1.,0.));
#11715=DIRECTION('ref_axis',(1.,0.,0.));
#11716=DIRECTION('center_axis',(0.,-1.,0.));
#11717=DIRECTION('ref_axis',(1.,0.,0.));
#11718=DIRECTION('',(0.707106781186548,0.707106781186547,8.65956056235493E-17));
#11719=DIRECTION('center_axis',(0.,-1.,0.));
#11720=DIRECTION('ref_axis',(1.,0.,0.));
#11721=DIRECTION('center_axis',(0.,-1.,0.));
#11722=DIRECTION('ref_axis',(1.,0.,0.));
#11723=DIRECTION('',(0.,1.,0.));
#11724=DIRECTION('center_axis',(0.,1.,0.));
#11725=DIRECTION('ref_axis',(1.,0.,0.));
#11726=DIRECTION('center_axis',(0.,-1.,0.));
#11727=DIRECTION('ref_axis',(1.,0.,0.));
#11728=DIRECTION('',(-0.707106781186547,0.707106781186548,-8.65956056235493E-17));
#11729=DIRECTION('center_axis',(0.,-1.,0.));
#11730=DIRECTION('ref_axis',(0.,0.,-1.));
#11731=DIRECTION('center_axis',(0.,-1.,0.));
#11732=DIRECTION('ref_axis',(1.,0.,0.));
#11733=DIRECTION('center_axis',(0.,1.,0.));
#11734=DIRECTION('ref_axis',(1.,0.,0.));
#11735=DIRECTION('center_axis',(0.,1.,0.));
#11736=DIRECTION('ref_axis',(1.,0.,0.));
#11737=DIRECTION('',(-0.447213595499958,0.894427190999916,-5.47678698264203E-17));
#11738=DIRECTION('center_axis',(0.,-1.,0.));
#11739=DIRECTION('ref_axis',(1.,0.,0.));
#11740=DIRECTION('',(0.,1.,0.));
#11741=DIRECTION('axis',(0.,0.,1.));
#11742=DIRECTION('refdir',(1.,0.,0.));
#11743=DIRECTION('center_axis',(0.866025403784439,0.,-0.5));
#11744=DIRECTION('ref_axis',(0.5,0.,0.866025403784439));
#11745=DIRECTION('',(-0.5,0.,-0.866025403784439));
#11746=DIRECTION('',(0.,-1.,0.));
#11747=DIRECTION('',(0.5,0.,0.866025403784439));
#11748=DIRECTION('',(0.,-1.,0.));
#11749=DIRECTION('center_axis',(1.60246890531964E-16,0.,-1.));
#11750=DIRECTION('ref_axis',(1.,0.,1.60246890531964E-16));
#11751=DIRECTION('',(-1.,0.,-1.60246890531964E-16));
#11752=DIRECTION('',(0.,-1.,0.));
#11753=DIRECTION('',(1.,0.,1.60246890531964E-16));
#11754=DIRECTION('center_axis',(-0.866025403784439,0.,-0.5));
#11755=DIRECTION('ref_axis',(0.5,0.,-0.866025403784439));
#11756=DIRECTION('',(-0.5,0.,0.866025403784439));
#11757=DIRECTION('',(0.,-1.,0.));
#11758=DIRECTION('',(0.5,0.,-0.866025403784439));
#11759=DIRECTION('center_axis',(-0.866025403784439,0.,0.5));
#11760=DIRECTION('ref_axis',(-0.5,0.,-0.866025403784439));
#11761=DIRECTION('',(0.5,0.,0.866025403784439));
#11762=DIRECTION('',(0.,-1.,0.));
#11763=DIRECTION('',(-0.5,0.,-0.866025403784439));
#11764=DIRECTION('center_axis',(-1.60246890531964E-16,0.,1.));
#11765=DIRECTION('ref_axis',(-1.,0.,-1.60246890531964E-16));
#11766=DIRECTION('',(1.,0.,1.60246890531964E-16));
#11767=DIRECTION('',(0.,-1.,0.));
#11768=DIRECTION('',(-1.,0.,-1.60246890531964E-16));
#11769=DIRECTION('center_axis',(0.866025403784439,0.,0.5));
#11770=DIRECTION('ref_axis',(-0.5,0.,0.866025403784439));
#11771=DIRECTION('',(0.5,0.,-0.866025403784439));
#11772=DIRECTION('',(-0.5,0.,0.866025403784439));
#11773=DIRECTION('center_axis',(0.,1.,0.));
#11774=DIRECTION('ref_axis',(1.,0.,0.));
#11775=DIRECTION('center_axis',(0.,-1.,0.));
#11776=DIRECTION('ref_axis',(0.,0.,-1.));
#11777=DIRECTION('center_axis',(0.,1.,0.));
#11778=DIRECTION('ref_axis',(1.,0.,0.));
#11779=DIRECTION('center_axis',(0.,1.,0.));
#11780=DIRECTION('ref_axis',(1.,0.,0.));
#11781=DIRECTION('center_axis',(0.,1.,0.));
#11782=DIRECTION('ref_axis',(0.,0.,1.));
#11783=DIRECTION('center_axis',(0.,-1.,0.));
#11784=DIRECTION('ref_axis',(1.,0.,0.));
#11785=DIRECTION('center_axis',(0.,-1.,0.));
#11786=DIRECTION('ref_axis',(1.,0.,0.));
#11787=DIRECTION('center_axis',(0.,-1.,0.));
#11788=DIRECTION('ref_axis',(1.,0.,0.));
#11789=DIRECTION('',(0.707106781186547,0.707106781186548,8.65956056235493E-17));
#11790=DIRECTION('center_axis',(0.,-1.,0.));
#11791=DIRECTION('ref_axis',(1.,0.,0.));
#11792=DIRECTION('center_axis',(0.,-1.,0.));
#11793=DIRECTION('ref_axis',(1.,0.,0.));
#11794=DIRECTION('',(0.,1.,0.));
#11795=DIRECTION('center_axis',(0.,1.,0.));
#11796=DIRECTION('ref_axis',(1.,0.,0.));
#11797=DIRECTION('center_axis',(0.,-1.,0.));
#11798=DIRECTION('ref_axis',(1.,0.,0.));
#11799=DIRECTION('',(-0.707106781186547,0.707106781186548,-8.65956056235493E-17));
#11800=DIRECTION('center_axis',(0.,-1.,0.));
#11801=DIRECTION('ref_axis',(0.,0.,-1.));
#11802=DIRECTION('center_axis',(0.,-1.,0.));
#11803=DIRECTION('ref_axis',(1.,0.,0.));
#11804=DIRECTION('center_axis',(0.,1.,0.));
#11805=DIRECTION('ref_axis',(1.,0.,0.));
#11806=DIRECTION('center_axis',(0.,1.,0.));
#11807=DIRECTION('ref_axis',(1.,0.,0.));
#11808=DIRECTION('',(-0.447213595499958,0.894427190999916,-5.47678698264203E-17));
#11809=DIRECTION('center_axis',(0.,-1.,0.));
#11810=DIRECTION('ref_axis',(1.,0.,0.));
#11811=DIRECTION('',(0.,1.,0.));
#11812=DIRECTION('',(0.,0.,1.));
#11813=DIRECTION('',(1.,0.,0.));
#11814=DIRECTION('',(0.,0.,1.));
#11815=DIRECTION('',(1.,0.,0.));
#11816=DIRECTION('',(0.,0.,1.));
#11817=DIRECTION('',(1.,0.,0.));
#11818=DIRECTION('',(0.,0.,1.));
#11819=DIRECTION('',(1.,0.,0.));
#11820=DIRECTION('',(0.,0.,1.));
#11821=DIRECTION('',(1.,0.,0.));
#11822=DIRECTION('',(0.,0.,1.));
#11823=DIRECTION('',(1.,0.,0.));
#11824=DIRECTION('',(0.,0.,1.));
#11825=DIRECTION('',(1.,0.,0.));
#11826=DIRECTION('',(0.,0.,1.));
#11827=DIRECTION('',(1.,0.,0.));
#11828=DIRECTION('',(0.,-1.,2.22044604925031E-16));
#11829=DIRECTION('',(1.,0.,0.));
#11830=DIRECTION('',(0.,-1.,2.22044604925031E-16));
#11831=DIRECTION('',(1.,0.,0.));
#11832=DIRECTION('',(0.,-1.,2.22044604925031E-16));
#11833=DIRECTION('',(1.,0.,0.));
#11834=DIRECTION('',(0.,-1.,2.22044604925031E-16));
#11835=DIRECTION('',(1.,0.,0.));
#11836=DIRECTION('',(0.,-1.,2.22044604925031E-16));
#11837=DIRECTION('',(1.,0.,0.));
#11838=DIRECTION('',(0.,-1.,2.22044604925031E-16));
#11839=DIRECTION('',(1.,0.,0.));
#11840=DIRECTION('',(0.,-1.,2.22044604925031E-16));
#11841=DIRECTION('',(1.,0.,0.));
#11842=DIRECTION('',(0.,-1.,2.22044604925031E-16));
#11843=DIRECTION('',(1.,0.,0.));
#11844=DIRECTION('',(0.,-1.,2.22044604925031E-16));
#11845=DIRECTION('',(1.,0.,0.));
#11846=DIRECTION('',(0.,-1.,2.22044604925031E-16));
#11847=DIRECTION('',(1.,0.,0.));
#11848=DIRECTION('',(0.,-1.,2.22044604925031E-16));
#11849=DIRECTION('',(1.,0.,0.));
#11850=DIRECTION('',(0.,-1.,2.22044604925031E-16));
#11851=DIRECTION('',(1.,0.,0.));
#11852=DIRECTION('',(0.,-1.,2.22044604925031E-16));
#11853=DIRECTION('',(1.,0.,0.));
#11854=DIRECTION('',(0.,-1.,2.22044604925031E-16));
#11855=DIRECTION('',(1.,0.,0.));
#11856=DIRECTION('',(0.,-1.,2.22044604925031E-16));
#11857=DIRECTION('',(1.,0.,0.));
#11858=DIRECTION('',(0.,-1.,2.22044604925031E-16));
#11859=DIRECTION('',(1.,0.,0.));
#11860=DIRECTION('',(0.,-1.,2.22044604925031E-16));
#11861=DIRECTION('',(1.,0.,0.));
#11862=DIRECTION('',(0.,-1.,2.22044604925031E-16));
#11863=DIRECTION('',(1.,0.,0.));
#11864=DIRECTION('',(0.,-1.,2.22044604925031E-16));
#11865=DIRECTION('',(1.,0.,0.));
#11866=DIRECTION('',(0.,-1.,2.22044604925031E-16));
#11867=DIRECTION('',(1.,0.,0.));
#11868=DIRECTION('',(0.,-1.,2.22044604925031E-16));
#11869=DIRECTION('',(1.,0.,0.));
#11870=DIRECTION('',(0.,-1.,2.22044604925031E-16));
#11871=DIRECTION('',(1.,0.,0.));
#11872=DIRECTION('',(0.,0.,1.));
#11873=DIRECTION('',(1.,0.,0.));
#11874=DIRECTION('',(0.,0.,1.));
#11875=DIRECTION('',(1.,0.,0.));
#11876=DIRECTION('',(0.,0.,1.));
#11877=DIRECTION('',(1.,0.,0.));
#11878=DIRECTION('',(0.,0.,1.));
#11879=DIRECTION('',(1.,0.,0.));
#11880=DIRECTION('',(0.,0.,1.));
#11881=DIRECTION('',(1.,0.,0.));
#11882=DIRECTION('',(0.,0.,1.));
#11883=DIRECTION('',(1.,0.,0.));
#11884=DIRECTION('',(0.,0.,1.));
#11885=DIRECTION('',(1.,0.,0.));
#11886=DIRECTION('',(0.,0.,1.));
#11887=DIRECTION('',(1.,0.,0.));
#11888=DIRECTION('',(0.,-1.,2.22044604925031E-16));
#11889=DIRECTION('',(1.,0.,0.));
#11890=DIRECTION('',(0.,0.,1.));
#11891=DIRECTION('',(2.22044604925031E-16,-1.,0.));
#11892=DIRECTION('',(0.,-1.,2.22044604925031E-16));
#11893=DIRECTION('',(1.,0.,0.));
#11894=DIRECTION('',(0.,0.,1.));
#11895=DIRECTION('',(1.,0.,0.));
#11896=DIRECTION('',(0.,0.,1.));
#11897=DIRECTION('',(1.,0.,0.));
#11898=DIRECTION('',(0.,0.,1.));
#11899=DIRECTION('',(1.,0.,0.));
#11900=DIRECTION('',(0.,0.,1.));
#11901=DIRECTION('',(1.,0.,0.));
#11902=DIRECTION('',(0.,0.,1.));
#11903=DIRECTION('',(1.,0.,0.));
#11904=DIRECTION('',(0.,0.,1.));
#11905=DIRECTION('',(1.,0.,0.));
#11906=DIRECTION('',(0.,0.,1.));
#11907=DIRECTION('',(1.,0.,0.));
#11908=DIRECTION('',(0.,0.,1.));
#11909=DIRECTION('',(2.22044604925031E-16,-1.,0.));
#11910=DIRECTION('',(0.,-1.,2.22044604925031E-16));
#11911=DIRECTION('',(1.,0.,0.));
#11912=DIRECTION('',(0.,0.,1.));
#11913=DIRECTION('',(1.,0.,0.));
#11914=DIRECTION('',(0.,0.,1.));
#11915=DIRECTION('',(1.,0.,0.));
#11916=DIRECTION('',(0.,0.,1.));
#11917=DIRECTION('',(1.,0.,0.));
#11918=DIRECTION('',(0.,0.,1.));
#11919=DIRECTION('',(1.,0.,0.));
#11920=DIRECTION('',(0.,0.,1.));
#11921=DIRECTION('',(1.,0.,0.));
#11922=DIRECTION('',(0.,0.,1.));
#11923=DIRECTION('',(1.,0.,0.));
#11924=DIRECTION('',(0.,-1.,2.22044604925031E-16));
#11925=DIRECTION('',(1.,0.,0.));
#11926=DIRECTION('',(0.,-1.,2.22044604925031E-16));
#11927=DIRECTION('',(1.,0.,0.));
#11928=DIRECTION('',(0.,-1.,2.22044604925031E-16));
#11929=DIRECTION('',(1.,0.,0.));
#11930=DIRECTION('',(0.,-1.,2.22044604925031E-16));
#11931=DIRECTION('',(1.,0.,0.));
#11932=DIRECTION('',(0.,-1.,2.22044604925031E-16));
#11933=DIRECTION('',(1.,0.,0.));
#11934=DIRECTION('',(0.,0.,1.));
#11935=DIRECTION('',(1.,0.,0.));
#11936=DIRECTION('',(0.,0.,1.));
#11937=DIRECTION('',(1.,0.,0.));
#11938=DIRECTION('',(0.,0.,1.));
#11939=DIRECTION('',(1.,0.,0.));
#11940=DIRECTION('',(0.,0.,1.));
#11941=DIRECTION('',(1.,0.,0.));
#11942=DIRECTION('',(0.,0.,1.));
#11943=DIRECTION('',(1.,0.,0.));
#11944=DIRECTION('',(0.,0.,1.));
#11945=DIRECTION('',(1.,0.,0.));
#11946=CARTESIAN_POINT('',(0.,0.,0.));
#11947=CARTESIAN_POINT('',(0.,0.,0.));
#11948=CARTESIAN_POINT('',(0.,0.,0.));
#11949=CARTESIAN_POINT('Origin',(-1.69705627484771,4.30294372515229,-0.1));
#11950=CARTESIAN_POINT('',(-1.90705627484771,4.30294372515229,0.));
#11951=CARTESIAN_POINT('Origin',(-1.69705627484771,4.30294372515229,0.));
#11952=CARTESIAN_POINT('',(-1.90705627484771,4.30294372515229,1.));
#11953=CARTESIAN_POINT('',(-1.90705627484771,4.30294372515229,-0.1));
#11954=CARTESIAN_POINT('Origin',(-1.69705627484771,4.30294372515229,1.));
#11955=CARTESIAN_POINT('Origin',(-1.69705627484771,7.69705627484771,-0.1));
#11956=CARTESIAN_POINT('',(-1.90705627484771,7.69705627484771,0.));
#11957=CARTESIAN_POINT('Origin',(-1.69705627484771,7.69705627484771,0.));
#11958=CARTESIAN_POINT('',(-1.90705627484771,7.69705627484771,1.));
#11959=CARTESIAN_POINT('',(-1.90705627484771,7.69705627484771,-0.1));
#11960=CARTESIAN_POINT('Origin',(-1.69705627484771,7.69705627484771,1.));
#11961=CARTESIAN_POINT('Origin',(1.69705627484771,7.69705627484771,-0.1));
#11962=CARTESIAN_POINT('',(1.48705627484771,7.69705627484771,0.));
#11963=CARTESIAN_POINT('Origin',(1.69705627484771,7.69705627484771,0.));
#11964=CARTESIAN_POINT('',(1.48705627484771,7.69705627484771,1.));
#11965=CARTESIAN_POINT('',(1.48705627484771,7.69705627484771,-0.1));
#11966=CARTESIAN_POINT('Origin',(1.69705627484771,7.69705627484771,1.));
#11967=CARTESIAN_POINT('Origin',(1.69705627484771,4.30294372515229,-0.1));
#11968=CARTESIAN_POINT('',(1.48705627484771,4.30294372515229,0.));
#11969=CARTESIAN_POINT('Origin',(1.69705627484771,4.30294372515229,0.));
#11970=CARTESIAN_POINT('',(1.48705627484771,4.30294372515229,1.));
#11971=CARTESIAN_POINT('',(1.48705627484771,4.30294372515229,-0.1));
#11972=CARTESIAN_POINT('Origin',(1.69705627484771,4.30294372515229,1.));
#11973=CARTESIAN_POINT('Origin',(-1.69705627484771,-1.69705627484771,-0.1));
#11974=CARTESIAN_POINT('',(-1.90705627484771,-1.69705627484771,0.));
#11975=CARTESIAN_POINT('Origin',(-1.69705627484771,-1.69705627484771,0.));
#11976=CARTESIAN_POINT('',(-1.90705627484771,-1.69705627484771,1.));
#11977=CARTESIAN_POINT('',(-1.90705627484771,-1.69705627484771,-0.1));
#11978=CARTESIAN_POINT('Origin',(-1.69705627484771,-1.69705627484771,1.));
#11979=CARTESIAN_POINT('Origin',(-1.69705627484771,1.69705627484771,-0.1));
#11980=CARTESIAN_POINT('',(-1.90705627484771,1.69705627484771,0.));
#11981=CARTESIAN_POINT('Origin',(-1.69705627484771,1.69705627484771,0.));
#11982=CARTESIAN_POINT('',(-1.90705627484771,1.69705627484771,1.));
#11983=CARTESIAN_POINT('',(-1.90705627484771,1.69705627484771,-0.1));
#11984=CARTESIAN_POINT('Origin',(-1.69705627484771,1.69705627484771,1.));
#11985=CARTESIAN_POINT('Origin',(1.69705627484771,1.69705627484771,-0.1));
#11986=CARTESIAN_POINT('',(1.48705627484771,1.69705627484771,0.));
#11987=CARTESIAN_POINT('Origin',(1.69705627484771,1.69705627484771,0.));
#11988=CARTESIAN_POINT('',(1.48705627484771,1.69705627484771,1.));
#11989=CARTESIAN_POINT('',(1.48705627484771,1.69705627484771,-0.1));
#11990=CARTESIAN_POINT('Origin',(1.69705627484771,1.69705627484771,1.));
#11991=CARTESIAN_POINT('Origin',(1.69705627484771,-1.69705627484771,-0.1));
#11992=CARTESIAN_POINT('',(1.48705627484771,-1.69705627484771,0.));
#11993=CARTESIAN_POINT('Origin',(1.69705627484771,-1.69705627484771,0.));
#11994=CARTESIAN_POINT('',(1.48705627484771,-1.69705627484771,1.));
#11995=CARTESIAN_POINT('',(1.48705627484771,-1.69705627484771,-0.1));
#11996=CARTESIAN_POINT('Origin',(1.69705627484771,-1.69705627484771,1.));
#11997=CARTESIAN_POINT('Origin',(18.5,16.,-0.1));
#11998=CARTESIAN_POINT('',(18.335,16.,0.));
#11999=CARTESIAN_POINT('Origin',(18.5,16.,0.));
#12000=CARTESIAN_POINT('',(18.335,16.,1.));
#12001=CARTESIAN_POINT('',(18.335,16.,-0.1));
#12002=CARTESIAN_POINT('Origin',(18.5,16.,1.));
#12003=CARTESIAN_POINT('Origin',(12.5,16.,-0.1));
#12004=CARTESIAN_POINT('',(12.335,16.,0.));
#12005=CARTESIAN_POINT('Origin',(12.5,16.,0.));
#12006=CARTESIAN_POINT('',(12.335,16.,1.));
#12007=CARTESIAN_POINT('',(12.335,16.,-0.1));
#12008=CARTESIAN_POINT('Origin',(12.5,16.,1.));
#12009=CARTESIAN_POINT('Origin',(6.5,16.,-0.1));
#12010=CARTESIAN_POINT('',(6.335,16.,0.));
#12011=CARTESIAN_POINT('Origin',(6.5,16.,0.));
#12012=CARTESIAN_POINT('',(6.335,16.,1.));
#12013=CARTESIAN_POINT('',(6.335,16.,-0.1));
#12014=CARTESIAN_POINT('Origin',(6.5,16.,1.));
#12015=CARTESIAN_POINT('Origin',(0.5,16.,-0.1));
#12016=CARTESIAN_POINT('',(0.335,16.,0.));
#12017=CARTESIAN_POINT('Origin',(0.5,16.,0.));
#12018=CARTESIAN_POINT('',(0.335,16.,1.));
#12019=CARTESIAN_POINT('',(0.335,16.,-0.1));
#12020=CARTESIAN_POINT('Origin',(0.5,16.,1.));
#12021=CARTESIAN_POINT('Origin',(21.,20.,0.));
#12022=CARTESIAN_POINT('',(21.,20.,0.));
#12023=CARTESIAN_POINT('',(-9.,20.,0.));
#12024=CARTESIAN_POINT('',(21.,20.,0.));
#12025=CARTESIAN_POINT('',(-9.,20.,1.));
#12026=CARTESIAN_POINT('',(-9.,20.,0.));
#12027=CARTESIAN_POINT('',(21.,20.,1.));
#12028=CARTESIAN_POINT('',(21.,20.,1.));
#12029=CARTESIAN_POINT('',(21.,20.,0.));
#12030=CARTESIAN_POINT('Origin',(21.,-3.5,0.));
#12031=CARTESIAN_POINT('',(21.,-3.5,0.));
#12032=CARTESIAN_POINT('',(21.,-3.5,0.));
#12033=CARTESIAN_POINT('',(21.,-3.5,1.));
#12034=CARTESIAN_POINT('',(21.,-3.5,1.));
#12035=CARTESIAN_POINT('',(21.,-3.5,0.));
#12036=CARTESIAN_POINT('Origin',(-9.,-3.5,0.));
#12037=CARTESIAN_POINT('',(-9.,-3.5,0.));
#12038=CARTESIAN_POINT('',(-9.,-3.5,0.));
#12039=CARTESIAN_POINT('',(-9.,-3.5,1.));
#12040=CARTESIAN_POINT('',(-9.,-3.5,1.));
#12041=CARTESIAN_POINT('',(-9.,-3.5,0.));
#12042=CARTESIAN_POINT('Origin',(-9.,20.,0.));
#12043=CARTESIAN_POINT('',(-9.,20.,0.));
#12044=CARTESIAN_POINT('',(-9.,20.,1.));
#12045=CARTESIAN_POINT('Origin',(6.,8.25,1.));
#12046=CARTESIAN_POINT('Origin',(6.,8.25,0.));
#12047=CARTESIAN_POINT('',(0.,0.,0.));
#12048=CARTESIAN_POINT('Origin',(-8.,20.,-0.8));
#12049=CARTESIAN_POINT('',(-8.,20.,-0.8));
#12050=CARTESIAN_POINT('',(-9.,20.,-0.8));
#12051=CARTESIAN_POINT('',(-8.,20.,-0.8));
#12052=CARTESIAN_POINT('',(-9.,20.,0.));
#12053=CARTESIAN_POINT('',(-9.,20.,-0.8));
#12054=CARTESIAN_POINT('',(-8.,20.,0.));
#12055=CARTESIAN_POINT('',(-8.,20.,0.));
#12056=CARTESIAN_POINT('',(-8.,20.,-0.8));
#12057=CARTESIAN_POINT('Origin',(-8.,-3.5,-0.8));
#12058=CARTESIAN_POINT('',(-8.,-3.5,-0.8));
#12059=CARTESIAN_POINT('',(-8.,-3.5,-0.8));
#12060=CARTESIAN_POINT('',(-8.,-3.5,0.));
#12061=CARTESIAN_POINT('',(-8.,-3.5,0.));
#12062=CARTESIAN_POINT('',(-8.,-3.5,-0.8));
#12063=CARTESIAN_POINT('Origin',(-9.,-3.5,-0.8));
#12064=CARTESIAN_POINT('',(-9.,-3.5,-0.8));
#12065=CARTESIAN_POINT('',(-9.,-3.5,-0.8));
#12066=CARTESIAN_POINT('',(-9.,-3.5,0.));
#12067=CARTESIAN_POINT('',(-9.,-3.5,0.));
#12068=CARTESIAN_POINT('',(-9.,-3.5,-0.8));
#12069=CARTESIAN_POINT('Origin',(-9.,20.,-0.8));
#12070=CARTESIAN_POINT('',(-9.,20.,-0.8));
#12071=CARTESIAN_POINT('',(-9.,20.,0.));
#12072=CARTESIAN_POINT('Origin',(-8.5,8.25,0.));
#12073=CARTESIAN_POINT('Origin',(-8.5,8.25,-0.8));
#12074=CARTESIAN_POINT('',(0.,0.,0.));
#12075=CARTESIAN_POINT('Origin',(21.,20.,-0.8));
#12076=CARTESIAN_POINT('',(21.,20.,-0.8));
#12077=CARTESIAN_POINT('',(20.,20.,-0.8));
#12078=CARTESIAN_POINT('',(21.,20.,-0.8));
#12079=CARTESIAN_POINT('',(20.,20.,0.));
#12080=CARTESIAN_POINT('',(20.,20.,-0.8));
#12081=CARTESIAN_POINT('',(21.,20.,0.));
#12082=CARTESIAN_POINT('',(21.,20.,0.));
#12083=CARTESIAN_POINT('',(21.,20.,-0.8));
#12084=CARTESIAN_POINT('Origin',(21.,-3.5,-0.8));
#12085=CARTESIAN_POINT('',(21.,-3.5,-0.8));
#12086=CARTESIAN_POINT('',(21.,-3.5,-0.8));
#12087=CARTESIAN_POINT('',(21.,-3.5,0.));
#12088=CARTESIAN_POINT('',(21.,-3.5,0.));
#12089=CARTESIAN_POINT('',(21.,-3.5,-0.8));
#12090=CARTESIAN_POINT('Origin',(20.,-3.5,-0.8));
#12091=CARTESIAN_POINT('',(20.,-3.5,-0.8));
#12092=CARTESIAN_POINT('',(20.,-3.5,-0.8));
#12093=CARTESIAN_POINT('',(20.,-3.5,0.));
#12094=CARTESIAN_POINT('',(20.,-3.5,0.));
#12095=CARTESIAN_POINT('',(20.,-3.5,-0.8));
#12096=CARTESIAN_POINT('Origin',(20.,20.,-0.8));
#12097=CARTESIAN_POINT('',(20.,20.,-0.8));
#12098=CARTESIAN_POINT('',(20.,20.,0.));
#12099=CARTESIAN_POINT('Origin',(20.5,8.25,0.));
#12100=CARTESIAN_POINT('Origin',(20.5,8.25,-0.8));
#12101=CARTESIAN_POINT('',(0.,0.,0.));
#12102=CARTESIAN_POINT('Origin',(0.9,0.,1.4));
#12103=CARTESIAN_POINT('',(0.988888264668966,0.25,1.4));
#12104=CARTESIAN_POINT('',(1.02,-1.18386380373883E-17,1.65));
#12105=CARTESIAN_POINT('Ctrl Pts',(0.988888264668966,0.25,1.4));
#12106=CARTESIAN_POINT('Ctrl Pts',(0.988888264668966,0.25,1.43153139415882));
#12107=CARTESIAN_POINT('Ctrl Pts',(0.990553370646674,0.243672048431404,
1.46507214966317));
#12108=CARTESIAN_POINT('Ctrl Pts',(0.996491737296663,0.218119830014375,
1.52662620974954));
#12109=CARTESIAN_POINT('Ctrl Pts',(1.00067109353237,0.198902128206072,1.5546512623872));
#12110=CARTESIAN_POINT('Ctrl Pts',(1.00845756932386,0.154654113568716,1.59889927702456));
#12111=CARTESIAN_POINT('Ctrl Pts',(1.01258144235289,0.126627870945253,1.61811920309393));
#12112=CARTESIAN_POINT('Ctrl Pts',(1.0183917429657,0.065069600391363,1.64367304400768));
#12113=CARTESIAN_POINT('Ctrl Pts',(1.02,0.031527330883376,1.65));
#12114=CARTESIAN_POINT('Ctrl Pts',(1.02,2.77555756156289E-17,1.65));
#12115=CARTESIAN_POINT('Ctrl Pts',(1.02,6.93889390390723E-18,1.65));
#12116=CARTESIAN_POINT('Ctrl Pts',(1.02,-0.031527330883376,1.65));
#12117=CARTESIAN_POINT('Ctrl Pts',(1.0183917429657,-0.065069600391363,1.64367304400768));
#12118=CARTESIAN_POINT('Ctrl Pts',(1.01258144235289,-0.126627870945253,
1.61811920309393));
#12119=CARTESIAN_POINT('Ctrl Pts',(1.00845756932386,-0.154654113568716,
1.59889927702456));
#12120=CARTESIAN_POINT('Ctrl Pts',(1.00067109353237,-0.198902128206072,
1.5546512623872));
#12121=CARTESIAN_POINT('Ctrl Pts',(0.996491737296663,-0.218119830014375,
1.52662620974954));
#12122=CARTESIAN_POINT('Ctrl Pts',(0.990553370646674,-0.243672048431404,
1.46507214966317));
#12123=CARTESIAN_POINT('Ctrl Pts',(0.988888264668967,-0.25,1.43153139415882));
#12124=CARTESIAN_POINT('Ctrl Pts',(0.988888264668967,-0.25,1.36846860584118));
#12125=CARTESIAN_POINT('Ctrl Pts',(0.990553370646674,-0.243672048431404,
1.33492785033683));
#12126=CARTESIAN_POINT('Ctrl Pts',(0.996491737296663,-0.218119830014375,
1.27337379025046));
#12127=CARTESIAN_POINT('Ctrl Pts',(1.00067109353237,-0.198902128206072,
1.2453487376128));
#12128=CARTESIAN_POINT('Ctrl Pts',(1.00845756932386,-0.154654113568716,
1.20110072297544));
#12129=CARTESIAN_POINT('Ctrl Pts',(1.01258144235289,-0.126627870945254,
1.18188079690607));
#12130=CARTESIAN_POINT('Ctrl Pts',(1.0183917429657,-0.0650696003913633,
1.15632695599232));
#12131=CARTESIAN_POINT('Ctrl Pts',(1.02,-0.0315273308833761,1.15));
#12132=CARTESIAN_POINT('Ctrl Pts',(1.02,0.0315273308833759,1.15));
#12133=CARTESIAN_POINT('Ctrl Pts',(1.0183917429657,0.065069600391363,1.15632695599232));
#12134=CARTESIAN_POINT('Ctrl Pts',(1.01258144235289,0.126627870945253,1.18188079690607));
#12135=CARTESIAN_POINT('Ctrl Pts',(1.00845756932386,0.154654113568716,1.20110072297544));
#12136=CARTESIAN_POINT('Ctrl Pts',(1.00067109353237,0.198902128206072,1.2453487376128));
#12137=CARTESIAN_POINT('Ctrl Pts',(0.996491737296663,0.218119830014375,
1.27337379025046));
#12138=CARTESIAN_POINT('Ctrl Pts',(0.990553370646674,0.243672048431404,
1.33492785033683));
#12139=CARTESIAN_POINT('Ctrl Pts',(0.988888264668967,0.25,1.36846860584118));
#12140=CARTESIAN_POINT('Ctrl Pts',(0.988888264668967,0.25,1.4));
#12141=CARTESIAN_POINT('',(2.9,-3.06161699786838E-17,1.65));
#12142=CARTESIAN_POINT('',(0.9,-3.06161699786838E-17,1.65));
#12143=CARTESIAN_POINT('',(2.88920404263873,0.25,1.4));
#12144=CARTESIAN_POINT('Ctrl Pts',(2.88920404263873,0.25,1.4));
#12145=CARTESIAN_POINT('Ctrl Pts',(2.88920404263873,0.25,1.36859268214333));
#12146=CARTESIAN_POINT('Ctrl Pts',(2.8897689135262,0.243720046736958,1.33510260402868));
#12147=CARTESIAN_POINT('Ctrl Pts',(2.89180770664292,0.218201792012593,1.27351240469396));
#12148=CARTESIAN_POINT('Ctrl Pts',(2.89325203146722,0.198964344197684,1.24541095360441));
#12149=CARTESIAN_POINT('Ctrl Pts',(2.89596207500507,0.154589088004924,1.20103569741165));
#12150=CARTESIAN_POINT('Ctrl Pts',(2.89740405468483,0.126487618562645,1.18179821727709));
#12151=CARTESIAN_POINT('Ctrl Pts',(2.89943748106926,0.0648973582672708,
1.15627993798745));
#12152=CARTESIAN_POINT('Ctrl Pts',(2.9,0.0314072589573412,1.15));
#12153=CARTESIAN_POINT('Ctrl Pts',(2.9,-0.0314072589573412,1.15));
#12154=CARTESIAN_POINT('Ctrl Pts',(2.89943748106926,-0.0648973582672708,
1.15627993798745));
#12155=CARTESIAN_POINT('Ctrl Pts',(2.89740405468483,-0.126487618562645,
1.18179821727709));
#12156=CARTESIAN_POINT('Ctrl Pts',(2.89596207500507,-0.154589088004924,
1.20103569741165));
#12157=CARTESIAN_POINT('Ctrl Pts',(2.89325203146722,-0.198964344197684,
1.24541095360441));
#12158=CARTESIAN_POINT('Ctrl Pts',(2.89180770664292,-0.218201792012593,
1.27351240469396));
#12159=CARTESIAN_POINT('Ctrl Pts',(2.8897689135262,-0.243720046736958,1.33510260402868));
#12160=CARTESIAN_POINT('Ctrl Pts',(2.88920404263873,-0.25,1.36859268214333));
#12161=CARTESIAN_POINT('Ctrl Pts',(2.88920404263873,-0.25,1.43140731785667));
#12162=CARTESIAN_POINT('Ctrl Pts',(2.8897689135262,-0.243720046736958,1.46489739597132));
#12163=CARTESIAN_POINT('Ctrl Pts',(2.89180770664292,-0.218201792012593,
1.52648759530604));
#12164=CARTESIAN_POINT('Ctrl Pts',(2.89325203146722,-0.198964344197684,
1.55458904639559));
#12165=CARTESIAN_POINT('Ctrl Pts',(2.89596207500507,-0.154589088004924,
1.59896430258835));
#12166=CARTESIAN_POINT('Ctrl Pts',(2.89740405468483,-0.126487618562645,
1.61820178272291));
#12167=CARTESIAN_POINT('Ctrl Pts',(2.89943748106926,-0.0648973582672709,
1.64372006201255));
#12168=CARTESIAN_POINT('Ctrl Pts',(2.9,-0.0314072589573412,1.65));
#12169=CARTESIAN_POINT('Ctrl Pts',(2.9,1.38777878078145E-17,1.65));
#12170=CARTESIAN_POINT('Ctrl Pts',(2.9,-2.08166817117217E-17,1.65));
#12171=CARTESIAN_POINT('Ctrl Pts',(2.9,0.0314072589573412,1.65));
#12172=CARTESIAN_POINT('Ctrl Pts',(2.89943748106926,0.0648973582672708,
1.64372006201255));
#12173=CARTESIAN_POINT('Ctrl Pts',(2.89740405468483,0.126487618562645,1.61820178272291));
#12174=CARTESIAN_POINT('Ctrl Pts',(2.89596207500507,0.154589088004924,1.59896430258835));
#12175=CARTESIAN_POINT('Ctrl Pts',(2.89325203146722,0.198964344197684,1.55458904639559));
#12176=CARTESIAN_POINT('Ctrl Pts',(2.89180770664292,0.218201792012593,1.52648759530604));
#12177=CARTESIAN_POINT('Ctrl Pts',(2.8897689135262,0.243720046736958,1.46489739597132));
#12178=CARTESIAN_POINT('Ctrl Pts',(2.88920404263873,0.25,1.43140731785667));
#12179=CARTESIAN_POINT('Ctrl Pts',(2.88920404263873,0.25,1.4));
#12180=CARTESIAN_POINT('Origin',(-1.23743686707646,-1.23743686707646,2.9));
#12181=CARTESIAN_POINT('',(-1.40243686707646,-1.23743686707646,2.9));
#12182=CARTESIAN_POINT('Origin',(-1.23743686707646,-1.23743686707646,2.9));
#12183=CARTESIAN_POINT('',(-1.40243686707646,-1.23743686707646,3.6));
#12184=CARTESIAN_POINT('',(-1.40243686707646,-1.23743686707646,2.9));
#12185=CARTESIAN_POINT('Origin',(-1.23743686707646,-1.23743686707646,3.6));
#12186=CARTESIAN_POINT('Origin',(-1.23743686707646,-1.23743686707646,2.9));
#12187=CARTESIAN_POINT('Origin',(-1.23743686707646,1.23743686707646,2.9));
#12188=CARTESIAN_POINT('',(-1.40243686707646,1.23743686707646,2.9));
#12189=CARTESIAN_POINT('Origin',(-1.23743686707646,1.23743686707646,2.9));
#12190=CARTESIAN_POINT('',(-1.40243686707646,1.23743686707646,3.6));
#12191=CARTESIAN_POINT('',(-1.40243686707646,1.23743686707646,2.9));
#12192=CARTESIAN_POINT('Origin',(-1.23743686707646,1.23743686707646,3.6));
#12193=CARTESIAN_POINT('Origin',(-1.23743686707646,1.23743686707646,2.9));
#12194=CARTESIAN_POINT('Origin',(1.23743686707646,1.23743686707646,2.9));
#12195=CARTESIAN_POINT('',(1.07243686707646,1.23743686707646,2.9));
#12196=CARTESIAN_POINT('Origin',(1.23743686707646,1.23743686707646,2.9));
#12197=CARTESIAN_POINT('',(1.07243686707646,1.23743686707646,3.6));
#12198=CARTESIAN_POINT('',(1.07243686707646,1.23743686707646,2.9));
#12199=CARTESIAN_POINT('Origin',(1.23743686707646,1.23743686707646,3.6));
#12200=CARTESIAN_POINT('Origin',(1.23743686707646,1.23743686707646,2.9));
#12201=CARTESIAN_POINT('Origin',(1.23743686707646,-1.23743686707646,2.9));
#12202=CARTESIAN_POINT('',(1.07243686707646,-1.23743686707646,2.9));
#12203=CARTESIAN_POINT('Origin',(1.23743686707646,-1.23743686707646,2.9));
#12204=CARTESIAN_POINT('',(1.07243686707646,-1.23743686707646,3.6));
#12205=CARTESIAN_POINT('',(1.07243686707646,-1.23743686707646,2.9));
#12206=CARTESIAN_POINT('Origin',(1.23743686707646,-1.23743686707646,3.6));
#12207=CARTESIAN_POINT('Origin',(1.23743686707646,-1.23743686707646,2.9));
#12208=CARTESIAN_POINT('Origin',(-1.69705627484771,-1.69705627484771,1.8));
#12209=CARTESIAN_POINT('',(-1.19413676298012,-1.84771139285857,2.4));
#12210=CARTESIAN_POINT('',(-1.19413676298012,-1.84771139285857,1.8));
#12211=CARTESIAN_POINT('',(-1.19413676298012,-1.84771139285857,1.8));
#12212=CARTESIAN_POINT('',(-1.84771139285857,-1.19413676298012,2.4));
#12213=CARTESIAN_POINT('Origin',(-1.69705627484771,-1.69705627484771,2.4));
#12214=CARTESIAN_POINT('',(-1.84771139285857,-1.19413676298012,1.8));
#12215=CARTESIAN_POINT('',(-1.84771139285857,-1.19413676298012,1.8));
#12216=CARTESIAN_POINT('Origin',(-1.69705627484771,-1.69705627484771,1.8));
#12217=CARTESIAN_POINT('Origin',(-1.69705627484771,-1.69705627484771,2.4));
#12218=CARTESIAN_POINT('Origin',(0.,0.,2.4));
#12219=CARTESIAN_POINT('Origin',(-1.69705627484771,1.69705627484771,1.8));
#12220=CARTESIAN_POINT('',(-1.84771139285857,1.19413676298012,2.4));
#12221=CARTESIAN_POINT('',(-1.84771139285857,1.19413676298012,1.8));
#12222=CARTESIAN_POINT('',(-1.84771139285857,1.19413676298012,1.8));
#12223=CARTESIAN_POINT('',(-1.19413676298012,1.84771139285857,2.4));
#12224=CARTESIAN_POINT('Origin',(-1.69705627484771,1.69705627484771,2.4));
#12225=CARTESIAN_POINT('',(-1.19413676298012,1.84771139285857,1.8));
#12226=CARTESIAN_POINT('',(-1.19413676298012,1.84771139285857,1.8));
#12227=CARTESIAN_POINT('Origin',(-1.69705627484771,1.69705627484771,1.8));
#12228=CARTESIAN_POINT('Origin',(-1.69705627484771,1.69705627484771,2.4));
#12229=CARTESIAN_POINT('Origin',(0.,0.,2.4));
#12230=CARTESIAN_POINT('Origin',(1.69705627484771,1.69705627484771,1.8));
#12231=CARTESIAN_POINT('',(1.19413676298012,1.84771139285857,2.4));
#12232=CARTESIAN_POINT('',(1.19413676298012,1.84771139285857,1.8));
#12233=CARTESIAN_POINT('',(1.19413676298012,1.84771139285857,1.8));
#12234=CARTESIAN_POINT('',(1.84771139285857,1.19413676298012,2.4));
#12235=CARTESIAN_POINT('Origin',(1.69705627484771,1.69705627484771,2.4));
#12236=CARTESIAN_POINT('',(1.84771139285857,1.19413676298012,1.8));
#12237=CARTESIAN_POINT('',(1.84771139285857,1.19413676298012,1.8));
#12238=CARTESIAN_POINT('Origin',(1.69705627484771,1.69705627484771,1.8));
#12239=CARTESIAN_POINT('Origin',(1.69705627484771,1.69705627484771,2.4));
#12240=CARTESIAN_POINT('Origin',(0.,0.,2.4));
#12241=CARTESIAN_POINT('Origin',(1.69705627484771,-1.69705627484771,1.8));
#12242=CARTESIAN_POINT('',(1.84771139285857,-1.19413676298012,2.4));
#12243=CARTESIAN_POINT('',(1.84771139285857,-1.19413676298012,1.8));
#12244=CARTESIAN_POINT('',(1.84771139285857,-1.19413676298012,1.8));
#12245=CARTESIAN_POINT('',(1.19413676298012,-1.84771139285857,2.4));
#12246=CARTESIAN_POINT('Origin',(1.69705627484771,-1.69705627484771,2.4));
#12247=CARTESIAN_POINT('',(1.19413676298012,-1.84771139285857,1.8));
#12248=CARTESIAN_POINT('',(1.19413676298012,-1.84771139285857,1.8));
#12249=CARTESIAN_POINT('Origin',(1.69705627484771,-1.69705627484771,1.8));
#12250=CARTESIAN_POINT('Origin',(1.69705627484771,-1.69705627484771,2.4));
#12251=CARTESIAN_POINT('Origin',(0.,0.,2.4));
#12252=CARTESIAN_POINT('Origin',(0.,0.,1.8));
#12253=CARTESIAN_POINT('',(-2.9,-3.55147571752732E-16,1.8));
#12254=CARTESIAN_POINT('Origin',(0.,0.,1.8));
#12255=CARTESIAN_POINT('',(-2.2,-2.69422295812418E-16,1.8));
#12256=CARTESIAN_POINT('Origin',(0.,0.,1.8));
#12257=CARTESIAN_POINT('Origin',(0.,0.,1.8));
#12258=CARTESIAN_POINT('Origin',(0.,0.,1.8));
#12259=CARTESIAN_POINT('Origin',(0.,0.,1.8));
#12260=CARTESIAN_POINT('Origin',(0.,0.,1.8));
#12261=CARTESIAN_POINT('',(-1.97205627484771,-1.69705627484771,1.8));
#12262=CARTESIAN_POINT('Origin',(-1.69705627484771,-1.69705627484771,1.8));
#12263=CARTESIAN_POINT('',(-1.97205627484771,1.69705627484771,1.8));
#12264=CARTESIAN_POINT('Origin',(-1.69705627484771,1.69705627484771,1.8));
#12265=CARTESIAN_POINT('',(1.42205627484771,1.69705627484771,1.8));
#12266=CARTESIAN_POINT('Origin',(1.69705627484771,1.69705627484771,1.8));
#12267=CARTESIAN_POINT('',(1.42205627484771,-1.69705627484771,1.8));
#12268=CARTESIAN_POINT('Origin',(1.69705627484771,-1.69705627484771,1.8));
#12269=CARTESIAN_POINT('Origin',(-1.69705627484771,-1.69705627484771,0.9));
#12270=CARTESIAN_POINT('',(-1.97205627484771,-1.69705627484771,1.));
#12271=CARTESIAN_POINT('Origin',(-1.69705627484771,-1.69705627484771,1.));
#12272=CARTESIAN_POINT('',(-1.97205627484771,-1.69705627484771,0.9));
#12273=CARTESIAN_POINT('Origin',(-1.69705627484771,1.69705627484771,0.9));
#12274=CARTESIAN_POINT('',(-1.97205627484771,1.69705627484771,1.));
#12275=CARTESIAN_POINT('Origin',(-1.69705627484771,1.69705627484771,1.));
#12276=CARTESIAN_POINT('',(-1.97205627484771,1.69705627484771,0.9));
#12277=CARTESIAN_POINT('Origin',(1.69705627484771,1.69705627484771,0.9));
#12278=CARTESIAN_POINT('',(1.42205627484771,1.69705627484771,1.));
#12279=CARTESIAN_POINT('Origin',(1.69705627484771,1.69705627484771,1.));
#12280=CARTESIAN_POINT('',(1.42205627484771,1.69705627484771,0.9));
#12281=CARTESIAN_POINT('Origin',(1.69705627484771,-1.69705627484771,0.9));
#12282=CARTESIAN_POINT('',(1.42205627484771,-1.69705627484771,1.));
#12283=CARTESIAN_POINT('Origin',(1.69705627484771,-1.69705627484771,1.));
#12284=CARTESIAN_POINT('',(1.42205627484771,-1.69705627484771,0.9));
#12285=CARTESIAN_POINT('Origin',(0.,0.,1.));
#12286=CARTESIAN_POINT('',(-2.2,-2.69422295812418E-16,3.6));
#12287=CARTESIAN_POINT('Origin',(0.,0.,3.6));
#12288=CARTESIAN_POINT('',(-2.2,-2.69422295812418E-16,1.));
#12289=CARTESIAN_POINT('Origin',(0.,0.,2.05));
#12290=CARTESIAN_POINT('',(-1.5,-1.83697019872103E-16,2.05));
#12291=CARTESIAN_POINT('Origin',(0.,0.,2.05));
#12292=CARTESIAN_POINT('',(-1.5,1.83697019872103E-16,3.6));
#12293=CARTESIAN_POINT('',(-1.5,-1.83697019872103E-16,2.05));
#12294=CARTESIAN_POINT('Origin',(0.,0.,3.6));
#12295=CARTESIAN_POINT('Origin',(0.,0.,2.05));
#12296=CARTESIAN_POINT('',(-1.02,-1.2491397351303E-16,2.05));
#12297=CARTESIAN_POINT('Origin',(0.,0.,2.05));
#12298=CARTESIAN_POINT('Origin',(0.,0.,1.));
#12299=CARTESIAN_POINT('',(-2.9,-3.55147571752732E-16,1.));
#12300=CARTESIAN_POINT('',(-2.9,-3.55147571752732E-16,1.));
#12301=CARTESIAN_POINT('Origin',(0.,0.,1.));
#12302=CARTESIAN_POINT('Origin',(0.,0.,1.));
#12303=CARTESIAN_POINT('',(-1.02,-1.2491397351303E-16,1.));
#12304=CARTESIAN_POINT('',(-1.02,-1.2491397351303E-16,1.));
#12305=CARTESIAN_POINT('Origin',(0.,0.,1.));
#12306=CARTESIAN_POINT('Origin',(0.,0.,3.6));
#12307=CARTESIAN_POINT('Origin',(0.,0.,1.));
#12308=CARTESIAN_POINT('',(0.,0.,0.));
#12309=CARTESIAN_POINT('Origin',(-1.23743686707646,-1.23743686707646,4.));
#12310=CARTESIAN_POINT('',(-1.61243686707646,-1.23743686707646,4.));
#12311=CARTESIAN_POINT('Origin',(-1.23743686707646,-1.23743686707646,4.));
#12312=CARTESIAN_POINT('',(-1.61243686707646,-1.23743686707646,4.4));
#12313=CARTESIAN_POINT('',(-1.61243686707646,-1.23743686707646,4.));
#12314=CARTESIAN_POINT('Origin',(-1.23743686707646,-1.23743686707646,4.4));
#12315=CARTESIAN_POINT('Origin',(-1.23743686707646,-1.23743686707646,4.));
#12316=CARTESIAN_POINT('',(-1.46243686707646,-1.23743686707646,4.));
#12317=CARTESIAN_POINT('Origin',(-1.23743686707646,-1.23743686707646,4.));
#12318=CARTESIAN_POINT('Origin',(-1.23743686707646,1.23743686707646,4.));
#12319=CARTESIAN_POINT('',(-1.61243686707646,1.23743686707646,4.));
#12320=CARTESIAN_POINT('Origin',(-1.23743686707646,1.23743686707646,4.));
#12321=CARTESIAN_POINT('',(-1.61243686707646,1.23743686707646,4.4));
#12322=CARTESIAN_POINT('',(-1.61243686707646,1.23743686707646,4.));
#12323=CARTESIAN_POINT('Origin',(-1.23743686707646,1.23743686707646,4.4));
#12324=CARTESIAN_POINT('Origin',(-1.23743686707646,1.23743686707646,4.));
#12325=CARTESIAN_POINT('',(-1.46243686707646,1.23743686707646,4.));
#12326=CARTESIAN_POINT('Origin',(-1.23743686707646,1.23743686707646,4.));
#12327=CARTESIAN_POINT('Origin',(1.23743686707646,1.23743686707646,4.));
#12328=CARTESIAN_POINT('',(0.862436867076458,1.23743686707646,4.));
#12329=CARTESIAN_POINT('Origin',(1.23743686707646,1.23743686707646,4.));
#12330=CARTESIAN_POINT('',(0.862436867076458,1.23743686707646,4.4));
#12331=CARTESIAN_POINT('',(0.862436867076458,1.23743686707646,4.));
#12332=CARTESIAN_POINT('Origin',(1.23743686707646,1.23743686707646,4.4));
#12333=CARTESIAN_POINT('Origin',(1.23743686707646,1.23743686707646,4.));
#12334=CARTESIAN_POINT('',(1.01243686707646,1.23743686707646,4.));
#12335=CARTESIAN_POINT('Origin',(1.23743686707646,1.23743686707646,4.));
#12336=CARTESIAN_POINT('Origin',(1.23743686707646,-1.23743686707646,4.));
#12337=CARTESIAN_POINT('',(0.862436867076458,-1.23743686707646,4.));
#12338=CARTESIAN_POINT('Origin',(1.23743686707646,-1.23743686707646,4.));
#12339=CARTESIAN_POINT('',(0.862436867076458,-1.23743686707646,4.4));
#12340=CARTESIAN_POINT('',(0.862436867076458,-1.23743686707646,4.));
#12341=CARTESIAN_POINT('Origin',(1.23743686707646,-1.23743686707646,4.4));
#12342=CARTESIAN_POINT('Origin',(1.23743686707646,-1.23743686707646,4.));
#12343=CARTESIAN_POINT('',(1.01243686707646,-1.23743686707646,4.));
#12344=CARTESIAN_POINT('Origin',(1.23743686707646,-1.23743686707646,4.));
#12345=CARTESIAN_POINT('Origin',(-1.23743686707646,-1.23743686707646,3.5));
#12346=CARTESIAN_POINT('',(-1.46243686707646,-1.23743686707646,3.6));
#12347=CARTESIAN_POINT('Origin',(-1.23743686707646,-1.23743686707646,3.6));
#12348=CARTESIAN_POINT('',(-1.46243686707646,-1.23743686707646,3.5));
#12349=CARTESIAN_POINT('Origin',(-1.23743686707646,1.23743686707646,3.5));
#12350=CARTESIAN_POINT('',(-1.46243686707646,1.23743686707646,3.6));
#12351=CARTESIAN_POINT('Origin',(-1.23743686707646,1.23743686707646,3.6));
#12352=CARTESIAN_POINT('',(-1.46243686707646,1.23743686707646,3.5));
#12353=CARTESIAN_POINT('Origin',(1.23743686707646,1.23743686707646,3.5));
#12354=CARTESIAN_POINT('',(1.01243686707646,1.23743686707646,3.6));
#12355=CARTESIAN_POINT('Origin',(1.23743686707646,1.23743686707646,3.6));
#12356=CARTESIAN_POINT('',(1.01243686707646,1.23743686707646,3.5));
#12357=CARTESIAN_POINT('Origin',(1.23743686707646,-1.23743686707646,3.5));
#12358=CARTESIAN_POINT('',(1.01243686707646,-1.23743686707646,3.6));
#12359=CARTESIAN_POINT('Origin',(1.23743686707646,-1.23743686707646,3.6));
#12360=CARTESIAN_POINT('',(1.01243686707646,-1.23743686707646,3.5));
#12361=CARTESIAN_POINT('Origin',(0.,0.,2.95));
#12362=CARTESIAN_POINT('',(-1.49,-1.82472373072956E-16,3.6));
#12363=CARTESIAN_POINT('Origin',(0.,0.,3.6));
#12364=CARTESIAN_POINT('',(-1.49,-1.82472373072956E-16,2.95));
#12365=CARTESIAN_POINT('',(-1.49,-1.82472373072956E-16,2.95));
#12366=CARTESIAN_POINT('Origin',(0.,0.,2.95));
#12367=CARTESIAN_POINT('Origin',(0.,0.,2.95));
#12368=CARTESIAN_POINT('',(-0.71,-8.69499227394621E-17,2.95));
#12369=CARTESIAN_POINT('Origin',(0.,0.,2.95));
#12370=CARTESIAN_POINT('Origin',(0.,0.,3.6));
#12371=CARTESIAN_POINT('',(-0.71,-8.69499227394621E-17,4.4));
#12372=CARTESIAN_POINT('Origin',(0.,0.,4.4));
#12373=CARTESIAN_POINT('',(-0.71,-8.69499227394621E-17,3.6));
#12374=CARTESIAN_POINT('Origin',(0.,0.,3.6));
#12375=CARTESIAN_POINT('',(-2.2,-2.69422295812418E-16,4.4));
#12376=CARTESIAN_POINT('Origin',(0.,0.,4.4));
#12377=CARTESIAN_POINT('',(-2.2,-2.69422295812418E-16,3.6));
#12378=CARTESIAN_POINT('',(-2.2,-2.69422295812418E-16,3.6));
#12379=CARTESIAN_POINT('Origin',(0.,0.,3.6));
#12380=CARTESIAN_POINT('Origin',(0.,0.,4.4));
#12381=CARTESIAN_POINT('Origin',(0.,0.,3.6));
#12382=CARTESIAN_POINT('',(0.,0.,0.));
#12383=CARTESIAN_POINT('Origin',(0.9,6.,1.4));
#12384=CARTESIAN_POINT('',(0.988888264668967,6.25,1.4));
#12385=CARTESIAN_POINT('',(1.02,6.,1.65));
#12386=CARTESIAN_POINT('Ctrl Pts',(0.988888264668967,6.25,1.4));
#12387=CARTESIAN_POINT('Ctrl Pts',(0.988888264668967,6.25,1.43153139415882));
#12388=CARTESIAN_POINT('Ctrl Pts',(0.990553370646674,6.2436720484314,1.46507214966317));
#12389=CARTESIAN_POINT('Ctrl Pts',(0.996491737296663,6.21811983001438,1.52662620974954));
#12390=CARTESIAN_POINT('Ctrl Pts',(1.00067109353237,6.19890212820607,1.5546512623872));
#12391=CARTESIAN_POINT('Ctrl Pts',(1.00845756932386,6.15465411356872,1.59889927702456));
#12392=CARTESIAN_POINT('Ctrl Pts',(1.01258144235289,6.12662787094525,1.61811920309393));
#12393=CARTESIAN_POINT('Ctrl Pts',(1.0183917429657,6.06506960039136,1.64367304400768));
#12394=CARTESIAN_POINT('Ctrl Pts',(1.02,6.03152733088338,1.65));
#12395=CARTESIAN_POINT('Ctrl Pts',(1.02,6.,1.65));
#12396=CARTESIAN_POINT('Ctrl Pts',(1.02,6.,1.65));
#12397=CARTESIAN_POINT('Ctrl Pts',(1.02,5.96847266911662,1.65));
#12398=CARTESIAN_POINT('Ctrl Pts',(1.0183917429657,5.93493039960864,1.64367304400768));
#12399=CARTESIAN_POINT('Ctrl Pts',(1.01258144235289,5.87337212905475,1.61811920309393));
#12400=CARTESIAN_POINT('Ctrl Pts',(1.00845756932386,5.84534588643128,1.59889927702456));
#12401=CARTESIAN_POINT('Ctrl Pts',(1.00067109353237,5.80109787179393,1.5546512623872));
#12402=CARTESIAN_POINT('Ctrl Pts',(0.996491737296663,5.78188016998562,1.52662620974954));
#12403=CARTESIAN_POINT('Ctrl Pts',(0.990553370646674,5.7563279515686,1.46507214966317));
#12404=CARTESIAN_POINT('Ctrl Pts',(0.988888264668967,5.75,1.43153139415882));
#12405=CARTESIAN_POINT('Ctrl Pts',(0.988888264668967,5.75,1.36846860584118));
#12406=CARTESIAN_POINT('Ctrl Pts',(0.990553370646674,5.7563279515686,1.33492785033683));
#12407=CARTESIAN_POINT('Ctrl Pts',(0.996491737296663,5.78188016998562,1.27337379025046));
#12408=CARTESIAN_POINT('Ctrl Pts',(1.00067109353237,5.80109787179393,1.2453487376128));
#12409=CARTESIAN_POINT('Ctrl Pts',(1.00845756932386,5.84534588643128,1.20110072297544));
#12410=CARTESIAN_POINT('Ctrl Pts',(1.01258144235289,5.87337212905475,1.18188079690607));
#12411=CARTESIAN_POINT('Ctrl Pts',(1.0183917429657,5.93493039960864,1.15632695599232));
#12412=CARTESIAN_POINT('Ctrl Pts',(1.02,5.96847266911662,1.15));
#12413=CARTESIAN_POINT('Ctrl Pts',(1.02,6.03152733088338,1.15));
#12414=CARTESIAN_POINT('Ctrl Pts',(1.0183917429657,6.06506960039136,1.15632695599232));
#12415=CARTESIAN_POINT('Ctrl Pts',(1.01258144235289,6.12662787094525,1.18188079690607));
#12416=CARTESIAN_POINT('Ctrl Pts',(1.00845756932386,6.15465411356872,1.20110072297544));
#12417=CARTESIAN_POINT('Ctrl Pts',(1.00067109353237,6.19890212820607,1.2453487376128));
#12418=CARTESIAN_POINT('Ctrl Pts',(0.996491737296663,6.21811983001438,1.27337379025046));
#12419=CARTESIAN_POINT('Ctrl Pts',(0.990553370646674,6.2436720484314,1.33492785033683));
#12420=CARTESIAN_POINT('Ctrl Pts',(0.988888264668967,6.25,1.36846860584118));
#12421=CARTESIAN_POINT('Ctrl Pts',(0.988888264668967,6.25,1.4));
#12422=CARTESIAN_POINT('',(2.9,6.,1.65));
#12423=CARTESIAN_POINT('',(0.9,6.,1.65));
#12424=CARTESIAN_POINT('',(2.88920404263873,6.25,1.4));
#12425=CARTESIAN_POINT('Ctrl Pts',(2.88920404263873,6.25,1.4));
#12426=CARTESIAN_POINT('Ctrl Pts',(2.88920404263873,6.25,1.36859268214333));
#12427=CARTESIAN_POINT('Ctrl Pts',(2.8897689135262,6.24372004673696,1.33510260402868));
#12428=CARTESIAN_POINT('Ctrl Pts',(2.89180770664292,6.21820179201259,1.27351240469396));
#12429=CARTESIAN_POINT('Ctrl Pts',(2.89325203146722,6.19896434419768,1.24541095360441));
#12430=CARTESIAN_POINT('Ctrl Pts',(2.89596207500507,6.15458908800492,1.20103569741165));
#12431=CARTESIAN_POINT('Ctrl Pts',(2.89740405468483,6.12648761856264,1.18179821727708));
#12432=CARTESIAN_POINT('Ctrl Pts',(2.89943748106926,6.06489735826727,1.15627993798745));
#12433=CARTESIAN_POINT('Ctrl Pts',(2.9,6.03140725895734,1.15));
#12434=CARTESIAN_POINT('Ctrl Pts',(2.9,5.96859274104266,1.15));
#12435=CARTESIAN_POINT('Ctrl Pts',(2.89943748106926,5.93510264173273,1.15627993798745));
#12436=CARTESIAN_POINT('Ctrl Pts',(2.89740405468483,5.87351238143735,1.18179821727708));
#12437=CARTESIAN_POINT('Ctrl Pts',(2.89596207500507,5.84541091199508,1.20103569741165));
#12438=CARTESIAN_POINT('Ctrl Pts',(2.89325203146722,5.80103565580232,1.24541095360441));
#12439=CARTESIAN_POINT('Ctrl Pts',(2.89180770664292,5.78179820798741,1.27351240469396));
#12440=CARTESIAN_POINT('Ctrl Pts',(2.8897689135262,5.75627995326304,1.33510260402868));
#12441=CARTESIAN_POINT('Ctrl Pts',(2.88920404263873,5.75,1.36859268214333));
#12442=CARTESIAN_POINT('Ctrl Pts',(2.88920404263873,5.75,1.43140731785667));
#12443=CARTESIAN_POINT('Ctrl Pts',(2.8897689135262,5.75627995326304,1.46489739597132));
#12444=CARTESIAN_POINT('Ctrl Pts',(2.89180770664292,5.78179820798741,1.52648759530604));
#12445=CARTESIAN_POINT('Ctrl Pts',(2.89325203146722,5.80103565580232,1.55458904639559));
#12446=CARTESIAN_POINT('Ctrl Pts',(2.89596207500507,5.84541091199508,1.59896430258835));
#12447=CARTESIAN_POINT('Ctrl Pts',(2.89740405468483,5.87351238143735,1.61820178272292));
#12448=CARTESIAN_POINT('Ctrl Pts',(2.89943748106926,5.93510264173273,1.64372006201255));
#12449=CARTESIAN_POINT('Ctrl Pts',(2.9,5.96859274104266,1.65));
#12450=CARTESIAN_POINT('Ctrl Pts',(2.9,6.,1.65));
#12451=CARTESIAN_POINT('Ctrl Pts',(2.9,6.,1.65));
#12452=CARTESIAN_POINT('Ctrl Pts',(2.9,6.03140725895734,1.65));
#12453=CARTESIAN_POINT('Ctrl Pts',(2.89943748106926,6.06489735826727,1.64372006201255));
#12454=CARTESIAN_POINT('Ctrl Pts',(2.89740405468483,6.12648761856265,1.61820178272292));
#12455=CARTESIAN_POINT('Ctrl Pts',(2.89596207500507,6.15458908800492,1.59896430258835));
#12456=CARTESIAN_POINT('Ctrl Pts',(2.89325203146722,6.19896434419768,1.55458904639559));
#12457=CARTESIAN_POINT('Ctrl Pts',(2.89180770664292,6.21820179201259,1.52648759530604));
#12458=CARTESIAN_POINT('Ctrl Pts',(2.8897689135262,6.24372004673696,1.46489739597132));
#12459=CARTESIAN_POINT('Ctrl Pts',(2.88920404263873,6.25,1.43140731785667));
#12460=CARTESIAN_POINT('Ctrl Pts',(2.88920404263873,6.25,1.4));
#12461=CARTESIAN_POINT('Origin',(-1.23743686707646,4.76256313292354,2.9));
#12462=CARTESIAN_POINT('',(-1.40243686707646,4.76256313292354,2.9));
#12463=CARTESIAN_POINT('Origin',(-1.23743686707646,4.76256313292354,2.9));
#12464=CARTESIAN_POINT('',(-1.40243686707646,4.76256313292354,3.6));
#12465=CARTESIAN_POINT('',(-1.40243686707646,4.76256313292354,2.9));
#12466=CARTESIAN_POINT('Origin',(-1.23743686707646,4.76256313292354,3.6));
#12467=CARTESIAN_POINT('Origin',(-1.23743686707646,4.76256313292354,2.9));
#12468=CARTESIAN_POINT('Origin',(-1.23743686707646,7.23743686707646,2.9));
#12469=CARTESIAN_POINT('',(-1.40243686707646,7.23743686707646,2.9));
#12470=CARTESIAN_POINT('Origin',(-1.23743686707646,7.23743686707646,2.9));
#12471=CARTESIAN_POINT('',(-1.40243686707646,7.23743686707646,3.6));
#12472=CARTESIAN_POINT('',(-1.40243686707646,7.23743686707646,2.9));
#12473=CARTESIAN_POINT('Origin',(-1.23743686707646,7.23743686707646,3.6));
#12474=CARTESIAN_POINT('Origin',(-1.23743686707646,7.23743686707646,2.9));
#12475=CARTESIAN_POINT('Origin',(1.23743686707646,7.23743686707646,2.9));
#12476=CARTESIAN_POINT('',(1.07243686707646,7.23743686707646,2.9));
#12477=CARTESIAN_POINT('Origin',(1.23743686707646,7.23743686707646,2.9));
#12478=CARTESIAN_POINT('',(1.07243686707646,7.23743686707646,3.6));
#12479=CARTESIAN_POINT('',(1.07243686707646,7.23743686707646,2.9));
#12480=CARTESIAN_POINT('Origin',(1.23743686707646,7.23743686707646,3.6));
#12481=CARTESIAN_POINT('Origin',(1.23743686707646,7.23743686707646,2.9));
#12482=CARTESIAN_POINT('Origin',(1.23743686707646,4.76256313292354,2.9));
#12483=CARTESIAN_POINT('',(1.07243686707646,4.76256313292354,2.9));
#12484=CARTESIAN_POINT('Origin',(1.23743686707646,4.76256313292354,2.9));
#12485=CARTESIAN_POINT('',(1.07243686707646,4.76256313292354,3.6));
#12486=CARTESIAN_POINT('',(1.07243686707646,4.76256313292354,2.9));
#12487=CARTESIAN_POINT('Origin',(1.23743686707646,4.76256313292354,3.6));
#12488=CARTESIAN_POINT('Origin',(1.23743686707646,4.76256313292354,2.9));
#12489=CARTESIAN_POINT('Origin',(-1.69705627484771,4.30294372515229,1.8));
#12490=CARTESIAN_POINT('',(-1.19413676298012,4.15228860714143,2.4));
#12491=CARTESIAN_POINT('',(-1.19413676298012,4.15228860714143,1.8));
#12492=CARTESIAN_POINT('',(-1.19413676298012,4.15228860714143,1.8));
#12493=CARTESIAN_POINT('',(-1.84771139285857,4.80586323701988,2.4));
#12494=CARTESIAN_POINT('Origin',(-1.69705627484771,4.30294372515229,2.4));
#12495=CARTESIAN_POINT('',(-1.84771139285857,4.80586323701988,1.8));
#12496=CARTESIAN_POINT('',(-1.84771139285857,4.80586323701988,1.8));
#12497=CARTESIAN_POINT('Origin',(-1.69705627484771,4.30294372515229,1.8));
#12498=CARTESIAN_POINT('Origin',(-1.69705627484771,4.30294372515229,2.4));
#12499=CARTESIAN_POINT('Origin',(0.,6.,2.4));
#12500=CARTESIAN_POINT('Origin',(-1.69705627484771,7.69705627484771,1.8));
#12501=CARTESIAN_POINT('',(-1.84771139285857,7.19413676298012,2.4));
#12502=CARTESIAN_POINT('',(-1.84771139285857,7.19413676298012,1.8));
#12503=CARTESIAN_POINT('',(-1.84771139285857,7.19413676298012,1.8));
#12504=CARTESIAN_POINT('',(-1.19413676298012,7.84771139285857,2.4));
#12505=CARTESIAN_POINT('Origin',(-1.69705627484771,7.69705627484771,2.4));
#12506=CARTESIAN_POINT('',(-1.19413676298012,7.84771139285857,1.8));
#12507=CARTESIAN_POINT('',(-1.19413676298012,7.84771139285857,1.8));
#12508=CARTESIAN_POINT('Origin',(-1.69705627484771,7.69705627484771,1.8));
#12509=CARTESIAN_POINT('Origin',(-1.69705627484771,7.69705627484771,2.4));
#12510=CARTESIAN_POINT('Origin',(0.,6.,2.4));
#12511=CARTESIAN_POINT('Origin',(1.69705627484771,7.69705627484771,1.8));
#12512=CARTESIAN_POINT('',(1.19413676298012,7.84771139285857,2.4));
#12513=CARTESIAN_POINT('',(1.19413676298012,7.84771139285857,1.8));
#12514=CARTESIAN_POINT('',(1.19413676298012,7.84771139285857,1.8));
#12515=CARTESIAN_POINT('',(1.84771139285857,7.19413676298012,2.4));
#12516=CARTESIAN_POINT('Origin',(1.69705627484771,7.69705627484771,2.4));
#12517=CARTESIAN_POINT('',(1.84771139285857,7.19413676298012,1.8));
#12518=CARTESIAN_POINT('',(1.84771139285857,7.19413676298012,1.8));
#12519=CARTESIAN_POINT('Origin',(1.69705627484771,7.69705627484771,1.8));
#12520=CARTESIAN_POINT('Origin',(1.69705627484771,7.69705627484771,2.4));
#12521=CARTESIAN_POINT('Origin',(0.,6.,2.4));
#12522=CARTESIAN_POINT('Origin',(1.69705627484771,4.30294372515229,1.8));
#12523=CARTESIAN_POINT('',(1.84771139285857,4.80586323701988,2.4));
#12524=CARTESIAN_POINT('',(1.84771139285857,4.80586323701988,1.8));
#12525=CARTESIAN_POINT('',(1.84771139285857,4.80586323701988,1.8));
#12526=CARTESIAN_POINT('',(1.19413676298012,4.15228860714143,2.4));
#12527=CARTESIAN_POINT('Origin',(1.69705627484771,4.30294372515229,2.4));
#12528=CARTESIAN_POINT('',(1.19413676298012,4.15228860714143,1.8));
#12529=CARTESIAN_POINT('',(1.19413676298012,4.15228860714143,1.8));
#12530=CARTESIAN_POINT('Origin',(1.69705627484771,4.30294372515229,1.8));
#12531=CARTESIAN_POINT('Origin',(1.69705627484771,4.30294372515229,2.4));
#12532=CARTESIAN_POINT('Origin',(0.,6.,2.4));
#12533=CARTESIAN_POINT('Origin',(0.,6.,1.8));
#12534=CARTESIAN_POINT('',(-2.9,6.,1.8));
#12535=CARTESIAN_POINT('Origin',(0.,6.,1.8));
#12536=CARTESIAN_POINT('',(-2.2,6.,1.8));
#12537=CARTESIAN_POINT('Origin',(0.,6.,1.8));
#12538=CARTESIAN_POINT('Origin',(0.,6.,1.8));
#12539=CARTESIAN_POINT('Origin',(0.,6.,1.8));
#12540=CARTESIAN_POINT('Origin',(0.,6.,1.8));
#12541=CARTESIAN_POINT('Origin',(0.,6.,1.8));
#12542=CARTESIAN_POINT('',(-1.97205627484771,4.30294372515229,1.8));
#12543=CARTESIAN_POINT('Origin',(-1.69705627484771,4.30294372515229,1.8));
#12544=CARTESIAN_POINT('',(-1.97205627484771,7.69705627484771,1.8));
#12545=CARTESIAN_POINT('Origin',(-1.69705627484771,7.69705627484771,1.8));
#12546=CARTESIAN_POINT('',(1.42205627484771,7.69705627484771,1.8));
#12547=CARTESIAN_POINT('Origin',(1.69705627484771,7.69705627484771,1.8));
#12548=CARTESIAN_POINT('',(1.42205627484771,4.30294372515229,1.8));
#12549=CARTESIAN_POINT('Origin',(1.69705627484771,4.30294372515229,1.8));
#12550=CARTESIAN_POINT('Origin',(-1.69705627484771,4.30294372515229,0.9));
#12551=CARTESIAN_POINT('',(-1.97205627484771,4.30294372515229,1.));
#12552=CARTESIAN_POINT('Origin',(-1.69705627484771,4.30294372515229,1.));
#12553=CARTESIAN_POINT('',(-1.97205627484771,4.30294372515229,0.9));
#12554=CARTESIAN_POINT('Origin',(-1.69705627484771,7.69705627484771,0.9));
#12555=CARTESIAN_POINT('',(-1.97205627484771,7.69705627484771,1.));
#12556=CARTESIAN_POINT('Origin',(-1.69705627484771,7.69705627484771,1.));
#12557=CARTESIAN_POINT('',(-1.97205627484771,7.69705627484771,0.9));
#12558=CARTESIAN_POINT('Origin',(1.69705627484771,7.69705627484771,0.9));
#12559=CARTESIAN_POINT('',(1.42205627484771,7.69705627484771,1.));
#12560=CARTESIAN_POINT('Origin',(1.69705627484771,7.69705627484771,1.));
#12561=CARTESIAN_POINT('',(1.42205627484771,7.69705627484771,0.9));
#12562=CARTESIAN_POINT('Origin',(1.69705627484771,4.30294372515229,0.9));
#12563=CARTESIAN_POINT('',(1.42205627484771,4.30294372515229,1.));
#12564=CARTESIAN_POINT('Origin',(1.69705627484771,4.30294372515229,1.));
#12565=CARTESIAN_POINT('',(1.42205627484771,4.30294372515229,0.9));
#12566=CARTESIAN_POINT('Origin',(0.,6.,1.));
#12567=CARTESIAN_POINT('',(-2.2,6.,3.6));
#12568=CARTESIAN_POINT('Origin',(0.,6.,3.6));
#12569=CARTESIAN_POINT('',(-2.2,6.,1.));
#12570=CARTESIAN_POINT('Origin',(0.,6.,2.05));
#12571=CARTESIAN_POINT('',(-1.5,6.,2.05));
#12572=CARTESIAN_POINT('Origin',(0.,6.,2.05));
#12573=CARTESIAN_POINT('',(-1.5,6.,3.6));
#12574=CARTESIAN_POINT('',(-1.5,6.,2.05));
#12575=CARTESIAN_POINT('Origin',(0.,6.,3.6));
#12576=CARTESIAN_POINT('Origin',(0.,6.,2.05));
#12577=CARTESIAN_POINT('',(-1.02,6.,2.05));
#12578=CARTESIAN_POINT('Origin',(0.,6.,2.05));
#12579=CARTESIAN_POINT('Origin',(0.,6.,1.));
#12580=CARTESIAN_POINT('',(-2.9,6.,1.));
#12581=CARTESIAN_POINT('',(-2.9,6.,1.));
#12582=CARTESIAN_POINT('Origin',(0.,6.,1.));
#12583=CARTESIAN_POINT('Origin',(0.,6.,1.));
#12584=CARTESIAN_POINT('',(-1.02,6.,1.));
#12585=CARTESIAN_POINT('',(-1.02,6.,1.));
#12586=CARTESIAN_POINT('Origin',(0.,6.,1.));
#12587=CARTESIAN_POINT('Origin',(0.,6.,3.6));
#12588=CARTESIAN_POINT('Origin',(0.,6.,1.));
#12589=CARTESIAN_POINT('',(0.,0.,0.));
#12590=CARTESIAN_POINT('Origin',(-1.23743686707646,4.76256313292354,4.));
#12591=CARTESIAN_POINT('',(-1.61243686707646,4.76256313292354,4.));
#12592=CARTESIAN_POINT('Origin',(-1.23743686707646,4.76256313292354,4.));
#12593=CARTESIAN_POINT('',(-1.61243686707646,4.76256313292354,4.4));
#12594=CARTESIAN_POINT('',(-1.61243686707646,4.76256313292354,4.));
#12595=CARTESIAN_POINT('Origin',(-1.23743686707646,4.76256313292354,4.4));
#12596=CARTESIAN_POINT('Origin',(-1.23743686707646,4.76256313292354,4.));
#12597=CARTESIAN_POINT('',(-1.46243686707646,4.76256313292354,4.));
#12598=CARTESIAN_POINT('Origin',(-1.23743686707646,4.76256313292354,4.));
#12599=CARTESIAN_POINT('Origin',(-1.23743686707646,7.23743686707646,4.));
#12600=CARTESIAN_POINT('',(-1.61243686707646,7.23743686707646,4.));
#12601=CARTESIAN_POINT('Origin',(-1.23743686707646,7.23743686707646,4.));
#12602=CARTESIAN_POINT('',(-1.61243686707646,7.23743686707646,4.4));
#12603=CARTESIAN_POINT('',(-1.61243686707646,7.23743686707646,4.));
#12604=CARTESIAN_POINT('Origin',(-1.23743686707646,7.23743686707646,4.4));
#12605=CARTESIAN_POINT('Origin',(-1.23743686707646,7.23743686707646,4.));
#12606=CARTESIAN_POINT('',(-1.46243686707646,7.23743686707646,4.));
#12607=CARTESIAN_POINT('Origin',(-1.23743686707646,7.23743686707646,4.));
#12608=CARTESIAN_POINT('Origin',(1.23743686707646,7.23743686707646,4.));
#12609=CARTESIAN_POINT('',(0.862436867076458,7.23743686707646,4.));
#12610=CARTESIAN_POINT('Origin',(1.23743686707646,7.23743686707646,4.));
#12611=CARTESIAN_POINT('',(0.862436867076458,7.23743686707646,4.4));
#12612=CARTESIAN_POINT('',(0.862436867076458,7.23743686707646,4.));
#12613=CARTESIAN_POINT('Origin',(1.23743686707646,7.23743686707646,4.4));
#12614=CARTESIAN_POINT('Origin',(1.23743686707646,7.23743686707646,4.));
#12615=CARTESIAN_POINT('',(1.01243686707646,7.23743686707646,4.));
#12616=CARTESIAN_POINT('Origin',(1.23743686707646,7.23743686707646,4.));
#12617=CARTESIAN_POINT('Origin',(1.23743686707646,4.76256313292354,4.));
#12618=CARTESIAN_POINT('',(0.862436867076458,4.76256313292354,4.));
#12619=CARTESIAN_POINT('Origin',(1.23743686707646,4.76256313292354,4.));
#12620=CARTESIAN_POINT('',(0.862436867076458,4.76256313292354,4.4));
#12621=CARTESIAN_POINT('',(0.862436867076458,4.76256313292354,4.));
#12622=CARTESIAN_POINT('Origin',(1.23743686707646,4.76256313292354,4.4));
#12623=CARTESIAN_POINT('Origin',(1.23743686707646,4.76256313292354,4.));
#12624=CARTESIAN_POINT('',(1.01243686707646,4.76256313292354,4.));
#12625=CARTESIAN_POINT('Origin',(1.23743686707646,4.76256313292354,4.));
#12626=CARTESIAN_POINT('Origin',(-1.23743686707646,4.76256313292354,3.5));
#12627=CARTESIAN_POINT('',(-1.46243686707646,4.76256313292354,3.6));
#12628=CARTESIAN_POINT('Origin',(-1.23743686707646,4.76256313292354,3.6));
#12629=CARTESIAN_POINT('',(-1.46243686707646,4.76256313292354,3.5));
#12630=CARTESIAN_POINT('Origin',(-1.23743686707646,7.23743686707646,3.5));
#12631=CARTESIAN_POINT('',(-1.46243686707646,7.23743686707646,3.6));
#12632=CARTESIAN_POINT('Origin',(-1.23743686707646,7.23743686707646,3.6));
#12633=CARTESIAN_POINT('',(-1.46243686707646,7.23743686707646,3.5));
#12634=CARTESIAN_POINT('Origin',(1.23743686707646,7.23743686707646,3.5));
#12635=CARTESIAN_POINT('',(1.01243686707646,7.23743686707646,3.6));
#12636=CARTESIAN_POINT('Origin',(1.23743686707646,7.23743686707646,3.6));
#12637=CARTESIAN_POINT('',(1.01243686707646,7.23743686707646,3.5));
#12638=CARTESIAN_POINT('Origin',(1.23743686707646,4.76256313292354,3.5));
#12639=CARTESIAN_POINT('',(1.01243686707646,4.76256313292354,3.6));
#12640=CARTESIAN_POINT('Origin',(1.23743686707646,4.76256313292354,3.6));
#12641=CARTESIAN_POINT('',(1.01243686707646,4.76256313292354,3.5));
#12642=CARTESIAN_POINT('Origin',(0.,6.,2.95));
#12643=CARTESIAN_POINT('',(-1.49,6.,3.6));
#12644=CARTESIAN_POINT('Origin',(0.,6.,3.6));
#12645=CARTESIAN_POINT('',(-1.49,6.,2.95));
#12646=CARTESIAN_POINT('',(-1.49,6.,2.95));
#12647=CARTESIAN_POINT('Origin',(0.,6.,2.95));
#12648=CARTESIAN_POINT('Origin',(0.,6.,2.95));
#12649=CARTESIAN_POINT('',(-0.71,6.,2.95));
#12650=CARTESIAN_POINT('Origin',(0.,6.,2.95));
#12651=CARTESIAN_POINT('Origin',(0.,6.,3.6));
#12652=CARTESIAN_POINT('',(-0.71,6.,4.4));
#12653=CARTESIAN_POINT('Origin',(0.,6.,4.4));
#12654=CARTESIAN_POINT('',(-0.71,6.,3.6));
#12655=CARTESIAN_POINT('Origin',(0.,6.,3.6));
#12656=CARTESIAN_POINT('',(-2.2,6.,4.4));
#12657=CARTESIAN_POINT('Origin',(0.,6.,4.4));
#12658=CARTESIAN_POINT('',(-2.2,6.,3.6));
#12659=CARTESIAN_POINT('',(-2.2,6.,3.6));
#12660=CARTESIAN_POINT('Origin',(0.,6.,3.6));
#12661=CARTESIAN_POINT('Origin',(0.,6.,4.4));
#12662=CARTESIAN_POINT('Origin',(0.,6.,3.6));
#12663=CARTESIAN_POINT('',(0.,0.,0.));
#12664=CARTESIAN_POINT('Origin',(14.,0.,0.97));
#12665=CARTESIAN_POINT('',(13.625,-4.59242549680257E-17,0.97));
#12666=CARTESIAN_POINT('Origin',(14.,0.,0.97));
#12667=CARTESIAN_POINT('',(13.625,4.59242549680257E-17,1.5));
#12668=CARTESIAN_POINT('',(13.625,-4.59242549680257E-17,0.97));
#12669=CARTESIAN_POINT('Origin',(14.,0.,1.5));
#12670=CARTESIAN_POINT('Origin',(14.,0.,0.97));
#12671=CARTESIAN_POINT('',(13.775,-2.75545529808154E-17,0.97));
#12672=CARTESIAN_POINT('Origin',(14.,0.,0.97));
#12673=CARTESIAN_POINT('Origin',(8.,0.,0.97));
#12674=CARTESIAN_POINT('',(7.625,-4.59242549680257E-17,0.97));
#12675=CARTESIAN_POINT('Origin',(8.,0.,0.97));
#12676=CARTESIAN_POINT('',(7.625,4.59242549680257E-17,1.5));
#12677=CARTESIAN_POINT('',(7.625,-4.59242549680257E-17,0.97));
#12678=CARTESIAN_POINT('Origin',(8.,0.,1.5));
#12679=CARTESIAN_POINT('Origin',(8.,0.,0.97));
#12680=CARTESIAN_POINT('',(7.775,-2.75545529808154E-17,0.97));
#12681=CARTESIAN_POINT('Origin',(8.,0.,0.97));
#12682=CARTESIAN_POINT('Origin',(2.,0.,0.97));
#12683=CARTESIAN_POINT('',(1.625,-4.59242549680257E-17,0.97));
#12684=CARTESIAN_POINT('Origin',(2.,0.,0.97));
#12685=CARTESIAN_POINT('',(1.625,4.59242549680257E-17,1.5));
#12686=CARTESIAN_POINT('',(1.625,-4.59242549680257E-17,0.97));
#12687=CARTESIAN_POINT('Origin',(2.,0.,1.5));
#12688=CARTESIAN_POINT('Origin',(2.,0.,0.97));
#12689=CARTESIAN_POINT('',(1.775,-2.75545529808155E-17,0.97));
#12690=CARTESIAN_POINT('Origin',(2.,0.,0.97));
#12691=CARTESIAN_POINT('Origin',(20.,0.,0.97));
#12692=CARTESIAN_POINT('',(19.625,-4.59242549680257E-17,0.97));
#12693=CARTESIAN_POINT('Origin',(20.,0.,0.97));
#12694=CARTESIAN_POINT('',(19.625,4.59242549680257E-17,1.5));
#12695=CARTESIAN_POINT('',(19.625,-4.59242549680257E-17,0.97));
#12696=CARTESIAN_POINT('Origin',(20.,0.,1.5));
#12697=CARTESIAN_POINT('Origin',(20.,0.,0.97));
#12698=CARTESIAN_POINT('',(19.775,-2.75545529808156E-17,0.97));
#12699=CARTESIAN_POINT('Origin',(20.,0.,0.97));
#12700=CARTESIAN_POINT('Origin',(14.,0.,-0.1));
#12701=CARTESIAN_POINT('',(13.775,-2.75545529808154E-17,0.));
#12702=CARTESIAN_POINT('Origin',(14.,0.,0.));
#12703=CARTESIAN_POINT('',(13.775,-2.75545529808154E-17,-0.1));
#12704=CARTESIAN_POINT('Origin',(8.,0.,-0.1));
#12705=CARTESIAN_POINT('',(7.775,-2.75545529808154E-17,0.));
#12706=CARTESIAN_POINT('Origin',(8.,0.,0.));
#12707=CARTESIAN_POINT('',(7.775,-2.75545529808154E-17,-0.1));
#12708=CARTESIAN_POINT('Origin',(2.,0.,-0.1));
#12709=CARTESIAN_POINT('',(1.775,-2.75545529808155E-17,0.));
#12710=CARTESIAN_POINT('Origin',(2.,0.,0.));
#12711=CARTESIAN_POINT('',(1.775,-2.75545529808155E-17,-0.1));
#12712=CARTESIAN_POINT('Origin',(20.,0.,-0.1));
#12713=CARTESIAN_POINT('',(19.775,-2.75545529808156E-17,0.));
#12714=CARTESIAN_POINT('Origin',(20.,0.,0.));
#12715=CARTESIAN_POINT('',(19.775,-2.75545529808156E-17,-0.1));
#12716=CARTESIAN_POINT('Origin',(0.,-0.53,1.));
#12717=CARTESIAN_POINT('',(0.,-0.53,1.));
#12718=CARTESIAN_POINT('',(0.,-0.75,0.85));
#12719=CARTESIAN_POINT('',(0.,-0.53,1.));
#12720=CARTESIAN_POINT('',(22.,-0.75,0.85));
#12721=CARTESIAN_POINT('',(0.,-0.75,0.85));
#12722=CARTESIAN_POINT('',(22.,-0.53,1.));
#12723=CARTESIAN_POINT('',(22.,-0.53,1.));
#12724=CARTESIAN_POINT('',(0.,-0.53,1.));
#12725=CARTESIAN_POINT('Origin',(0.,-0.53,1.15));
#12726=CARTESIAN_POINT('',(0.,-0.53,1.15));
#12727=CARTESIAN_POINT('',(0.,-0.53,1.15));
#12728=CARTESIAN_POINT('',(22.,-0.53,1.15));
#12729=CARTESIAN_POINT('',(22.,-0.53,1.15));
#12730=CARTESIAN_POINT('',(0.,-0.53,1.15));
#12731=CARTESIAN_POINT('Origin',(0.,-0.75,1.3));
#12732=CARTESIAN_POINT('',(0.,-0.75,1.3));
#12733=CARTESIAN_POINT('',(0.,-0.75,1.3));
#12734=CARTESIAN_POINT('',(22.,-0.75,1.3));
#12735=CARTESIAN_POINT('',(22.,-0.75,1.3));
#12736=CARTESIAN_POINT('',(0.,-0.75,1.3));
#12737=CARTESIAN_POINT('Origin',(0.,-0.75,1.5));
#12738=CARTESIAN_POINT('',(0.,-0.75,1.5));
#12739=CARTESIAN_POINT('',(0.,-0.75,1.5));
#12740=CARTESIAN_POINT('',(22.,-0.75,1.5));
#12741=CARTESIAN_POINT('',(22.,-0.75,1.5));
#12742=CARTESIAN_POINT('',(0.,-0.75,1.5));
#12743=CARTESIAN_POINT('Origin',(0.,0.75,1.5));
#12744=CARTESIAN_POINT('',(0.,0.75,1.5));
#12745=CARTESIAN_POINT('',(0.,0.75,1.5));
#12746=CARTESIAN_POINT('',(22.,0.75,1.5));
#12747=CARTESIAN_POINT('',(22.,0.75,1.5));
#12748=CARTESIAN_POINT('',(0.,0.75,1.5));
#12749=CARTESIAN_POINT('Origin',(0.,0.75,1.3));
#12750=CARTESIAN_POINT('',(0.,0.75,1.3));
#12751=CARTESIAN_POINT('',(0.,0.75,1.3));
#12752=CARTESIAN_POINT('',(22.,0.75,1.3));
#12753=CARTESIAN_POINT('',(22.,0.75,1.3));
#12754=CARTESIAN_POINT('',(0.,0.75,1.3));
#12755=CARTESIAN_POINT('Origin',(0.,0.53,1.15));
#12756=CARTESIAN_POINT('',(0.,0.53,1.15));
#12757=CARTESIAN_POINT('',(0.,0.53,1.15));
#12758=CARTESIAN_POINT('',(22.,0.53,1.15));
#12759=CARTESIAN_POINT('',(22.,0.53,1.15));
#12760=CARTESIAN_POINT('',(0.,0.53,1.15));
#12761=CARTESIAN_POINT('Origin',(0.,0.53,1.));
#12762=CARTESIAN_POINT('',(0.,0.53,1.));
#12763=CARTESIAN_POINT('',(0.,0.53,1.));
#12764=CARTESIAN_POINT('',(22.,0.53,1.));
#12765=CARTESIAN_POINT('',(22.,0.53,1.));
#12766=CARTESIAN_POINT('',(0.,0.53,1.));
#12767=CARTESIAN_POINT('Origin',(0.,0.75,0.85));
#12768=CARTESIAN_POINT('',(0.,0.75,0.85));
#12769=CARTESIAN_POINT('',(0.,0.75,0.85));
#12770=CARTESIAN_POINT('',(22.,0.75,0.85));
#12771=CARTESIAN_POINT('',(22.,0.75,0.85));
#12772=CARTESIAN_POINT('',(0.,0.75,0.85));
#12773=CARTESIAN_POINT('Origin',(0.,0.75,0.));
#12774=CARTESIAN_POINT('',(0.,0.75,0.));
#12775=CARTESIAN_POINT('',(0.,0.75,0.));
#12776=CARTESIAN_POINT('',(22.,0.75,0.));
#12777=CARTESIAN_POINT('',(22.,0.75,0.));
#12778=CARTESIAN_POINT('',(0.,0.75,0.));
#12779=CARTESIAN_POINT('Origin',(0.,-0.75,0.));
#12780=CARTESIAN_POINT('',(0.,-0.75,0.));
#12781=CARTESIAN_POINT('',(0.,-0.75,0.));
#12782=CARTESIAN_POINT('',(22.,-0.75,0.));
#12783=CARTESIAN_POINT('',(22.,-0.75,0.));
#12784=CARTESIAN_POINT('',(0.,-0.75,0.));
#12785=CARTESIAN_POINT('Origin',(0.,-0.75,0.85));
#12786=CARTESIAN_POINT('',(0.,-0.75,0.85));
#12787=CARTESIAN_POINT('',(22.,-0.75,0.85));
#12788=CARTESIAN_POINT('Origin',(22.,0.,0.75));
#12789=CARTESIAN_POINT('Origin',(0.,0.,0.75));
#12790=CARTESIAN_POINT('',(0.,0.,0.));
#12791=CARTESIAN_POINT('',(0.,0.,0.));
#12792=CARTESIAN_POINT('Origin',(0.,0.,0.));
#12793=CARTESIAN_POINT('',(-0.976185,-0.246528389340863,-1.19548183562566E-16));
#12794=CARTESIAN_POINT('',(-1.19548183562566E-16,-0.246528389340863,0.976185));
#12795=CARTESIAN_POINT('Origin',(0.,-0.246528389340863,0.));
#12796=CARTESIAN_POINT('Origin',(0.,-0.246528389340863,0.));
#12797=CARTESIAN_POINT('',(-1.19548183562566E-16,0.246528389340863,0.976185));
#12798=CARTESIAN_POINT('Origin',(-1.22464679914735E-16,0.,1.));
#12799=CARTESIAN_POINT('',(-0.976185,0.246528389340863,1.19548183562566E-16));
#12800=CARTESIAN_POINT('Origin',(0.,0.246528389340863,0.));
#12801=CARTESIAN_POINT('Origin',(0.,0.246528389340863,0.));
#12802=CARTESIAN_POINT('Origin',(0.,0.,0.));
#12803=CARTESIAN_POINT('',(-0.976185,0.45,-1.19548183562566E-16));
#12804=CARTESIAN_POINT('',(-0.976185,0.,-1.19548183562566E-16));
#12805=CARTESIAN_POINT('Origin',(0.,0.45,0.));
#12806=CARTESIAN_POINT('Origin',(0.,0.,0.));
#12807=CARTESIAN_POINT('',(-0.5,-0.39,-6.12323399573677E-17));
#12808=CARTESIAN_POINT('Origin',(0.,-0.39,0.));
#12809=CARTESIAN_POINT('',(-0.5,0.39,-6.12323399573677E-17));
#12810=CARTESIAN_POINT('',(-0.5,0.,-6.12323399573677E-17));
#12811=CARTESIAN_POINT('Origin',(0.,0.39,0.));
#12812=CARTESIAN_POINT('Origin',(0.,0.42,0.));
#12813=CARTESIAN_POINT('',(-0.56,0.45,-6.85802207522518E-17));
#12814=CARTESIAN_POINT('',(-0.53,0.42,-6.49062803548097E-17));
#12815=CARTESIAN_POINT('Origin',(0.,0.45,0.));
#12816=CARTESIAN_POINT('Origin',(0.976185,0.45,0.));
#12817=CARTESIAN_POINT('Origin',(0.,0.,0.));
#12818=CARTESIAN_POINT('',(-0.976185,-0.45,-1.19548183562566E-16));
#12819=CARTESIAN_POINT('Origin',(0.,-0.45,0.));
#12820=CARTESIAN_POINT('',(-0.976185,0.,-1.19548183562566E-16));
#12821=CARTESIAN_POINT('Origin',(0.56,-0.45,0.));
#12822=CARTESIAN_POINT('',(-0.56,-0.45,-6.85802207522518E-17));
#12823=CARTESIAN_POINT('Origin',(0.,-0.45,0.));
#12824=CARTESIAN_POINT('Origin',(0.,-0.42,0.));
#12825=CARTESIAN_POINT('',(-0.53,-0.42,-6.49062803548097E-17));
#12826=CARTESIAN_POINT('',(0.,0.,0.));
#12827=CARTESIAN_POINT('Origin',(0.,0.,0.));
#12828=CARTESIAN_POINT('',(-1.023815,0.246528389340863,-1.25381176266905E-16));
#12829=CARTESIAN_POINT('',(-1.25381176266905E-16,0.246528389340863,1.023815));
#12830=CARTESIAN_POINT('Origin',(0.,0.246528389340863,0.));
#12831=CARTESIAN_POINT('Origin',(0.,0.246528389340863,0.));
#12832=CARTESIAN_POINT('',(-1.25381176266905E-16,-0.246528389340863,1.023815));
#12833=CARTESIAN_POINT('Origin',(-1.22464679914735E-16,0.,1.));
#12834=CARTESIAN_POINT('',(-1.023815,-0.246528389340863,1.25381176266905E-16));
#12835=CARTESIAN_POINT('Origin',(0.,-0.246528389340863,0.));
#12836=CARTESIAN_POINT('Origin',(0.,-0.246528389340863,0.));
#12837=CARTESIAN_POINT('Origin',(0.,0.,0.));
#12838=CARTESIAN_POINT('',(-1.023815,-0.45,-1.25381176266905E-16));
#12839=CARTESIAN_POINT('Origin',(0.,-0.45,0.));
#12840=CARTESIAN_POINT('',(-1.023815,0.,-1.25381176266905E-16));
#12841=CARTESIAN_POINT('Origin',(1.44,0.45,0.));
#12842=CARTESIAN_POINT('',(-1.44,0.45,-1.76349139077219E-16));
#12843=CARTESIAN_POINT('Origin',(0.,0.45,0.));
#12844=CARTESIAN_POINT('',(-1.023815,0.45,-1.25381176266905E-16));
#12845=CARTESIAN_POINT('Origin',(0.,0.45,0.));
#12846=CARTESIAN_POINT('Origin',(0.,0.42,0.));
#12847=CARTESIAN_POINT('',(-1.5,0.39,-1.83697019872103E-16));
#12848=CARTESIAN_POINT('Origin',(0.,0.39,0.));
#12849=CARTESIAN_POINT('',(-1.47,0.42,-1.80023079474661E-16));
#12850=CARTESIAN_POINT('Origin',(0.,0.,0.));
#12851=CARTESIAN_POINT('',(-1.5,-0.39,-1.83697019872103E-16));
#12852=CARTESIAN_POINT('Origin',(0.,-0.39,0.));
#12853=CARTESIAN_POINT('',(-1.5,0.,-1.83697019872103E-16));
#12854=CARTESIAN_POINT('Origin',(0.,-0.42,0.));
#12855=CARTESIAN_POINT('',(-1.44,-0.45,-1.76349139077219E-16));
#12856=CARTESIAN_POINT('Origin',(0.,-0.45,0.));
#12857=CARTESIAN_POINT('',(-1.47,-0.42,-1.80023079474661E-16));
#12858=CARTESIAN_POINT('Origin',(1.023815,-0.45,0.));
#12859=CARTESIAN_POINT('Origin',(0.,0.,0.));
#12860=CARTESIAN_POINT('',(-1.023815,0.,-1.25381176266905E-16));
#12861=CARTESIAN_POINT('',(0.,0.,0.));
#12862=CARTESIAN_POINT('Origin',(1.,0.,0.));
#12863=CARTESIAN_POINT('',(1.,-1.78583896120461E-33,0.23815));
#12864=CARTESIAN_POINT('',(1.,-1.78583896120461E-33,-0.23815));
#12865=CARTESIAN_POINT('Origin',(1.,0.,0.));
#12866=CARTESIAN_POINT('Origin',(0.707106781186548,0.,-0.707106781186547));
#12867=CARTESIAN_POINT('',(0.875504261126124,-1.78583896120461E-33,-0.538709301246971));
#12868=CARTESIAN_POINT('',(0.538709301246971,-1.78583896120461E-33,-0.875504261126124));
#12869=CARTESIAN_POINT('Origin',(0.707106781186548,0.,-0.707106781186547));
#12870=CARTESIAN_POINT('Origin',(6.12323399573677E-17,0.,-1.));
#12871=CARTESIAN_POINT('',(0.23815,-1.78583896120461E-33,-1.));
#12872=CARTESIAN_POINT('',(-0.23815,-1.78583896120461E-33,-1.));
#12873=CARTESIAN_POINT('Origin',(6.12323399573677E-17,0.,-1.));
#12874=CARTESIAN_POINT('Origin',(-0.707106781186547,0.,-0.707106781186548));
#12875=CARTESIAN_POINT('',(-0.538709301246971,-1.78583896120461E-33,-0.875504261126124));
#12876=CARTESIAN_POINT('',(-0.875504261126124,-1.78583896120461E-33,-0.538709301246971));
#12877=CARTESIAN_POINT('Origin',(-0.707106781186547,0.,-0.707106781186548));
#12878=CARTESIAN_POINT('Origin',(-1.,0.,-1.22464679914735E-16));
#12879=CARTESIAN_POINT('',(-1.,-1.78583896120461E-33,-0.23815));
#12880=CARTESIAN_POINT('',(-1.,-1.78583896120461E-33,0.23815));
#12881=CARTESIAN_POINT('Origin',(-1.,0.,-1.22464679914735E-16));
#12882=CARTESIAN_POINT('Origin',(-0.707106781186548,0.,0.707106781186547));
#12883=CARTESIAN_POINT('',(-0.875504261126124,-7.94881478324376E-33,0.538709301246971));
#12884=CARTESIAN_POINT('',(-0.538709301246971,4.37713686083455E-33,0.875504261126124));
#12885=CARTESIAN_POINT('Origin',(-0.707106781186548,0.,0.707106781186547));
#12886=CARTESIAN_POINT('Origin',(-1.83697019872103E-16,0.,1.));
#12887=CARTESIAN_POINT('',(-0.23815,-1.78583896120461E-33,1.));
#12888=CARTESIAN_POINT('',(0.23815,-1.78583896120461E-33,1.));
#12889=CARTESIAN_POINT('Origin',(-1.83697019872103E-16,0.,1.));
#12890=CARTESIAN_POINT('Origin',(0.707106781186547,0.,0.707106781186548));
#12891=CARTESIAN_POINT('',(0.538709301246971,-4.86732687222419E-33,0.875504261126124));
#12892=CARTESIAN_POINT('',(0.875504261126124,1.29564894981497E-33,0.538709301246971));
#12893=CARTESIAN_POINT('Origin',(0.707106781186547,0.,0.707106781186548));
#12894=CARTESIAN_POINT('',(0.,0.,0.));
#12895=CARTESIAN_POINT('Origin',(0.707106781186547,0.,0.707106781186548));
#12896=CARTESIAN_POINT('',(0.504455939115715,-0.04763,0.841298510752802));
#12897=CARTESIAN_POINT('',(0.841298510752802,-0.04763,0.504455939115715));
#12898=CARTESIAN_POINT('Ctrl Pts',(0.504455939115715,-0.04763,0.841298510752802));
#12899=CARTESIAN_POINT('Ctrl Pts',(0.508899795931835,-0.0740444353928835,
0.838633903678357));
#12900=CARTESIAN_POINT('Ctrl Pts',(0.517157748491652,-0.0999305678883309,
0.833661031856294));
#12901=CARTESIAN_POINT('Ctrl Pts',(0.537715343527944,-0.142345102874864,
0.820511285096538));
#12902=CARTESIAN_POINT('Ctrl Pts',(0.548874290046456,-0.159766064500479,
0.813159949759));
#12903=CARTESIAN_POINT('Ctrl Pts',(0.573915184558107,-0.190326085855194,
0.795684265985089));
#12904=CARTESIAN_POINT('Ctrl Pts',(0.587792702767295,-0.203463743702801,
0.78555112003688));
#12905=CARTESIAN_POINT('Ctrl Pts',(0.615966552324775,-0.224161999508995,
0.763642258217233));
#12906=CARTESIAN_POINT('Ctrl Pts',(0.631684198665438,-0.232861760990032,
0.750785745543687));
#12907=CARTESIAN_POINT('Ctrl Pts',(0.663382628119203,-0.244251601209411,
0.722929908501543));
#12908=CARTESIAN_POINT('Ctrl Pts',(0.679352081686668,-0.246942143572133,
0.707917883896095));
#12909=CARTESIAN_POINT('Ctrl Pts',(0.707917883896095,-0.246942143572133,
0.679352081686668));
#12910=CARTESIAN_POINT('Ctrl Pts',(0.722929908501543,-0.244251601209411,
0.663382628119203));
#12911=CARTESIAN_POINT('Ctrl Pts',(0.750785745543687,-0.232861760990032,
0.631684198665439));
#12912=CARTESIAN_POINT('Ctrl Pts',(0.763642258217232,-0.224161999508995,
0.615966552324775));
#12913=CARTESIAN_POINT('Ctrl Pts',(0.78555112003688,-0.203463743702801,
0.587792702767295));
#12914=CARTESIAN_POINT('Ctrl Pts',(0.795684265985088,-0.190326085855194,
0.573915184558108));
#12915=CARTESIAN_POINT('Ctrl Pts',(0.813159949759,-0.15976606450048,0.548874290046456));
#12916=CARTESIAN_POINT('Ctrl Pts',(0.820511285096538,-0.142345102874864,
0.537715343527944));
#12917=CARTESIAN_POINT('Ctrl Pts',(0.833661031856294,-0.099930567888331,
0.517157748491653));
#12918=CARTESIAN_POINT('Ctrl Pts',(0.838633903678357,-0.0740444353928835,
0.508899795931835));
#12919=CARTESIAN_POINT('Ctrl Pts',(0.841298510752801,-0.0476299999999999,
0.504455939115715));
#12920=CARTESIAN_POINT('',(0.528110872004958,-0.04763,0.871530771444223));
#12921=CARTESIAN_POINT('Origin',(0.707106781186547,-0.04763,0.707106781186548));
#12922=CARTESIAN_POINT('',(0.871530771444223,-0.04763,0.528110872004959));
#12923=CARTESIAN_POINT('Ctrl Pts',(0.871530771444223,-0.0476300000000001,
0.528110872004958));
#12924=CARTESIAN_POINT('Ctrl Pts',(0.87014664509073,-0.0609922781173483,
0.530395067942936));
#12925=CARTESIAN_POINT('Ctrl Pts',(0.868149331745851,-0.0742967091364493,
0.533674141594226));
#12926=CARTESIAN_POINT('Ctrl Pts',(0.85981294420286,-0.115492077056649,
0.54708917182331));
#12927=CARTESIAN_POINT('Ctrl Pts',(0.850993704737257,-0.141695629206859,
0.560922177770136));
#12928=CARTESIAN_POINT('Ctrl Pts',(0.830754510485543,-0.181890537957859,
0.590422647829571));
#12929=CARTESIAN_POINT('Ctrl Pts',(0.816896541396381,-0.201072148666545,
0.609616703125488));
#12930=CARTESIAN_POINT('Ctrl Pts',(0.792310597819928,-0.223955109275652,
0.641117951819998));
#12931=CARTESIAN_POINT('Ctrl Pts',(0.779109323683612,-0.232742381310829,
0.657208095763053));
#12932=CARTESIAN_POINT('Ctrl Pts',(0.750552691816206,-0.244234834628584,
0.68964083160521));
#12933=CARTESIAN_POINT('Ctrl Pts',(0.735185187071673,-0.246942143572133,
0.705971972091755));
#12934=CARTESIAN_POINT('Ctrl Pts',(0.705971972091754,-0.246942143572133,
0.735185187071673));
#12935=CARTESIAN_POINT('Ctrl Pts',(0.689640831605209,-0.244234834628584,
0.750552691816206));
#12936=CARTESIAN_POINT('Ctrl Pts',(0.657208095763052,-0.232742381310829,
0.779109323683612));
#12937=CARTESIAN_POINT('Ctrl Pts',(0.641117951819998,-0.223955109275652,
0.792310597819928));
#12938=CARTESIAN_POINT('Ctrl Pts',(0.609616703125487,-0.201072148666545,
0.816896541396382));
#12939=CARTESIAN_POINT('Ctrl Pts',(0.590422647829571,-0.181890537957858,
0.830754510485544));
#12940=CARTESIAN_POINT('Ctrl Pts',(0.560922177770135,-0.141695629206858,
0.850993704737257));
#12941=CARTESIAN_POINT('Ctrl Pts',(0.547089171823309,-0.115492077056649,
0.859812944202861));
#12942=CARTESIAN_POINT('Ctrl Pts',(0.533674141594226,-0.0742967091364491,
0.868149331745852));
#12943=CARTESIAN_POINT('Ctrl Pts',(0.530395067942936,-0.0609922781173483,
0.870146645090731));
#12944=CARTESIAN_POINT('Ctrl Pts',(0.528110872004958,-0.0476300000000001,
0.871530771444223));
#12945=CARTESIAN_POINT('Origin',(0.707106781186547,-0.04763,0.707106781186548));
#12946=CARTESIAN_POINT('Origin',(0.,-0.166705,0.));
#12947=CARTESIAN_POINT('',(0.242834539687906,-0.04763,0.989696097314));
#12948=CARTESIAN_POINT('Origin',(0.,-0.04763,0.));
#12949=CARTESIAN_POINT('',(-0.242834539687907,-0.04763,0.989696097314));
#12950=CARTESIAN_POINT('Ctrl Pts',(0.242834539687906,-0.04763,0.989696097314));
#12951=CARTESIAN_POINT('Ctrl Pts',(0.24024064412003,-0.0609922781173483,
0.990332542620729));
#12952=CARTESIAN_POINT('Ctrl Pts',(0.236509675094874,-0.0742967091364492,
0.991238884025248));
#12953=CARTESIAN_POINT('Ctrl Pts',(0.221129100087819,-0.115492077056649,
0.994830026707808));
#12954=CARTESIAN_POINT('Ctrl Pts',(0.205111543747588,-0.141695629206859,
0.998375294985966));
#12955=CARTESIAN_POINT('Ctrl Pts',(0.169940289819232,-0.181890537957859,
1.00492400591205));
#12956=CARTESIAN_POINT('Ctrl Pts',(0.1465689792446,-0.201072148666545,1.00869718865384));
#12957=CARTESIAN_POINT('Ctrl Pts',(0.106909345252087,-0.223955109275652,
1.01358704779679));
#12958=CARTESIAN_POINT('Ctrl Pts',(0.0861971848975941,-0.232742381310829,
1.0156297872271));
#12959=CARTESIAN_POINT('Ctrl Pts',(0.0430711894098822,-0.244234834628584,
1.01837060663223));
#12960=CARTESIAN_POINT('Ctrl Pts',(0.0206568624125605,-0.246942143572133,
1.019052));
#12961=CARTESIAN_POINT('Ctrl Pts',(-0.0206568624125608,-0.246942143572133,
1.019052));
#12962=CARTESIAN_POINT('Ctrl Pts',(-0.0430711894098825,-0.244234834628584,
1.01837060663223));
#12963=CARTESIAN_POINT('Ctrl Pts',(-0.0861971848975943,-0.232742381310829,
1.0156297872271));
#12964=CARTESIAN_POINT('Ctrl Pts',(-0.106909345252088,-0.223955109275652,
1.01358704779679));
#12965=CARTESIAN_POINT('Ctrl Pts',(-0.1465689792446,-0.201072148666545,
1.00869718865384));
#12966=CARTESIAN_POINT('Ctrl Pts',(-0.169940289819232,-0.181890537957859,
1.00492400591205));
#12967=CARTESIAN_POINT('Ctrl Pts',(-0.205111543747588,-0.141695629206859,
0.998375294985966));
#12968=CARTESIAN_POINT('Ctrl Pts',(-0.221129100087819,-0.115492077056649,
0.994830026707808));
#12969=CARTESIAN_POINT('Ctrl Pts',(-0.236509675094875,-0.0742967091364493,
0.991238884025248));
#12970=CARTESIAN_POINT('Ctrl Pts',(-0.24024064412003,-0.0609922781173483,
0.990332542620729));
#12971=CARTESIAN_POINT('Ctrl Pts',(-0.242834539687907,-0.04763,0.989696097314));
#12972=CARTESIAN_POINT('',(-0.528110872004959,-0.04763,0.871530771444223));
#12973=CARTESIAN_POINT('Origin',(0.,-0.04763,0.));
#12974=CARTESIAN_POINT('',(-0.871530771444223,-0.04763,0.528110872004958));
#12975=CARTESIAN_POINT('Ctrl Pts',(-0.528110872004958,-0.0476300000000001,
0.871530771444223));
#12976=CARTESIAN_POINT('Ctrl Pts',(-0.530395067942936,-0.0609922781173484,
0.87014664509073));
#12977=CARTESIAN_POINT('Ctrl Pts',(-0.533674141594226,-0.0742967091364493,
0.868149331745851));
#12978=CARTESIAN_POINT('Ctrl Pts',(-0.54708917182331,-0.115492077056649,
0.85981294420286));
#12979=CARTESIAN_POINT('Ctrl Pts',(-0.560922177770136,-0.141695629206859,
0.850993704737257));
#12980=CARTESIAN_POINT('Ctrl Pts',(-0.590422647829571,-0.181890537957859,
0.830754510485543));
#12981=CARTESIAN_POINT('Ctrl Pts',(-0.609616703125488,-0.201072148666545,
0.816896541396381));
#12982=CARTESIAN_POINT('Ctrl Pts',(-0.641117951819998,-0.223955109275652,
0.792310597819928));
#12983=CARTESIAN_POINT('Ctrl Pts',(-0.657208095763053,-0.232742381310829,
0.779109323683611));
#12984=CARTESIAN_POINT('Ctrl Pts',(-0.68964083160521,-0.244234834628584,
0.750552691816205));
#12985=CARTESIAN_POINT('Ctrl Pts',(-0.705971972091755,-0.246942143572133,
0.735185187071673));
#12986=CARTESIAN_POINT('Ctrl Pts',(-0.735185187071673,-0.246942143572133,
0.705971972091754));
#12987=CARTESIAN_POINT('Ctrl Pts',(-0.750552691816206,-0.244234834628584,
0.689640831605209));
#12988=CARTESIAN_POINT('Ctrl Pts',(-0.779109323683612,-0.232742381310829,
0.657208095763052));
#12989=CARTESIAN_POINT('Ctrl Pts',(-0.792310597819928,-0.223955109275652,
0.641117951819998));
#12990=CARTESIAN_POINT('Ctrl Pts',(-0.816896541396382,-0.201072148666545,
0.609616703125487));
#12991=CARTESIAN_POINT('Ctrl Pts',(-0.830754510485544,-0.181890537957858,
0.590422647829571));
#12992=CARTESIAN_POINT('Ctrl Pts',(-0.850993704737257,-0.141695629206858,
0.560922177770135));
#12993=CARTESIAN_POINT('Ctrl Pts',(-0.859812944202861,-0.115492077056649,
0.547089171823309));
#12994=CARTESIAN_POINT('Ctrl Pts',(-0.868149331745852,-0.0742967091364491,
0.533674141594226));
#12995=CARTESIAN_POINT('Ctrl Pts',(-0.870146645090731,-0.0609922781173483,
0.530395067942936));
#12996=CARTESIAN_POINT('Ctrl Pts',(-0.871530771444223,-0.04763,0.528110872004958));
#12997=CARTESIAN_POINT('',(-0.989696097314,-0.04763,0.242834539687906));
#12998=CARTESIAN_POINT('Origin',(0.,-0.04763,0.));
#12999=CARTESIAN_POINT('',(-1.019052,-0.246942143572133,1.248489836334E-16));
#13000=CARTESIAN_POINT('Ctrl Pts',(-0.989696097314,-0.04763,0.242834539687906));
#13001=CARTESIAN_POINT('Ctrl Pts',(-0.990332542620729,-0.0609922781173483,
0.24024064412003));
#13002=CARTESIAN_POINT('Ctrl Pts',(-0.991238884025248,-0.0742967091364492,
0.236509675094874));
#13003=CARTESIAN_POINT('Ctrl Pts',(-0.994830026707808,-0.115492077056649,
0.221129100087819));
#13004=CARTESIAN_POINT('Ctrl Pts',(-0.998375294985966,-0.141695629206859,
0.205111543747588));
#13005=CARTESIAN_POINT('Ctrl Pts',(-1.00492400591205,-0.181890537957859,
0.169940289819232));
#13006=CARTESIAN_POINT('Ctrl Pts',(-1.00869718865384,-0.201072148666545,
0.1465689792446));
#13007=CARTESIAN_POINT('Ctrl Pts',(-1.01358704779679,-0.223955109275652,
0.106909345252088));
#13008=CARTESIAN_POINT('Ctrl Pts',(-1.0156297872271,-0.232742381310829,
0.0861971848975944));
#13009=CARTESIAN_POINT('Ctrl Pts',(-1.01837060663223,-0.244234834628584,
0.0430711894098825));
#13010=CARTESIAN_POINT('Ctrl Pts',(-1.019052,-0.246942143572133,0.0206568624125608));
#13011=CARTESIAN_POINT('Ctrl Pts',(-1.019052,-0.246942143572133,1.2490009027033E-16));
#13012=CARTESIAN_POINT('',(-1.019052,-0.28578,1.24797876996471E-16));
#13013=CARTESIAN_POINT('',(-1.019052,-0.166705,1.24797876996471E-16));
#13014=CARTESIAN_POINT('Origin',(0.,-0.28578,0.));
#13015=CARTESIAN_POINT('',(-0.989696097314,-0.04763,-0.242834539687906));
#13016=CARTESIAN_POINT('Ctrl Pts',(-1.019052,-0.246942143572133,1.2490009027033E-16));
#13017=CARTESIAN_POINT('Ctrl Pts',(-1.019052,-0.246942143572133,-0.0206568624125605));
#13018=CARTESIAN_POINT('Ctrl Pts',(-1.01837060663223,-0.244234834628584,
-0.0430711894098822));
#13019=CARTESIAN_POINT('Ctrl Pts',(-1.0156297872271,-0.232742381310829,
-0.0861971848975941));
#13020=CARTESIAN_POINT('Ctrl Pts',(-1.01358704779679,-0.223955109275652,
-0.106909345252087));
#13021=CARTESIAN_POINT('Ctrl Pts',(-1.00869718865384,-0.201072148666546,
-0.1465689792446));
#13022=CARTESIAN_POINT('Ctrl Pts',(-1.00492400591205,-0.181890537957859,
-0.169940289819232));
#13023=CARTESIAN_POINT('Ctrl Pts',(-0.998375294985966,-0.141695629206859,
-0.205111543747588));
#13024=CARTESIAN_POINT('Ctrl Pts',(-0.994830026707808,-0.11549207705665,
-0.221129100087819));
#13025=CARTESIAN_POINT('Ctrl Pts',(-0.991238884025248,-0.0742967091364495,
-0.236509675094874));
#13026=CARTESIAN_POINT('Ctrl Pts',(-0.990332542620729,-0.0609922781173484,
-0.24024064412003));
#13027=CARTESIAN_POINT('Ctrl Pts',(-0.989696097314,-0.0476300000000001,
-0.242834539687907));
#13028=CARTESIAN_POINT('',(-0.871530771444223,-0.04763,-0.528110872004958));
#13029=CARTESIAN_POINT('Origin',(0.,-0.04763,0.));
#13030=CARTESIAN_POINT('',(-0.528110872004958,-0.04763,-0.871530771444223));
#13031=CARTESIAN_POINT('Ctrl Pts',(-0.871530771444223,-0.0476300000000001,
-0.528110872004958));
#13032=CARTESIAN_POINT('Ctrl Pts',(-0.87014664509073,-0.0609922781173484,
-0.530395067942936));
#13033=CARTESIAN_POINT('Ctrl Pts',(-0.868149331745851,-0.0742967091364494,
-0.533674141594226));
#13034=CARTESIAN_POINT('Ctrl Pts',(-0.85981294420286,-0.115492077056649,
-0.54708917182331));
#13035=CARTESIAN_POINT('Ctrl Pts',(-0.850993704737257,-0.141695629206859,
-0.560922177770136));
#13036=CARTESIAN_POINT('Ctrl Pts',(-0.830754510485543,-0.181890537957859,
-0.590422647829571));
#13037=CARTESIAN_POINT('Ctrl Pts',(-0.816896541396381,-0.201072148666546,
-0.609616703125488));
#13038=CARTESIAN_POINT('Ctrl Pts',(-0.792310597819928,-0.223955109275652,
-0.641117951819999));
#13039=CARTESIAN_POINT('Ctrl Pts',(-0.779109323683611,-0.232742381310829,
-0.657208095763053));
#13040=CARTESIAN_POINT('Ctrl Pts',(-0.750552691816205,-0.244234834628584,
-0.68964083160521));
#13041=CARTESIAN_POINT('Ctrl Pts',(-0.735185187071673,-0.246942143572133,
-0.705971972091755));
#13042=CARTESIAN_POINT('Ctrl Pts',(-0.705971972091754,-0.246942143572133,
-0.735185187071673));
#13043=CARTESIAN_POINT('Ctrl Pts',(-0.68964083160521,-0.244234834628584,
-0.750552691816206));
#13044=CARTESIAN_POINT('Ctrl Pts',(-0.657208095763052,-0.232742381310829,
-0.779109323683612));
#13045=CARTESIAN_POINT('Ctrl Pts',(-0.641117951819998,-0.223955109275652,
-0.792310597819928));
#13046=CARTESIAN_POINT('Ctrl Pts',(-0.609616703125488,-0.201072148666545,
-0.816896541396381));
#13047=CARTESIAN_POINT('Ctrl Pts',(-0.590422647829571,-0.181890537957859,
-0.830754510485543));
#13048=CARTESIAN_POINT('Ctrl Pts',(-0.560922177770136,-0.141695629206859,
-0.850993704737257));
#13049=CARTESIAN_POINT('Ctrl Pts',(-0.54708917182331,-0.115492077056649,
-0.85981294420286));
#13050=CARTESIAN_POINT('Ctrl Pts',(-0.533674141594226,-0.0742967091364494,
-0.868149331745852));
#13051=CARTESIAN_POINT('Ctrl Pts',(-0.530395067942936,-0.0609922781173484,
-0.870146645090731));
#13052=CARTESIAN_POINT('Ctrl Pts',(-0.528110872004958,-0.0476300000000001,
-0.871530771444223));
#13053=CARTESIAN_POINT('',(-0.242834539687906,-0.04763,-0.989696097314));
#13054=CARTESIAN_POINT('Origin',(0.,-0.04763,0.));
#13055=CARTESIAN_POINT('',(0.242834539687906,-0.04763,-0.989696097314));
#13056=CARTESIAN_POINT('Ctrl Pts',(-0.242834539687907,-0.04763,-0.989696097314));
#13057=CARTESIAN_POINT('Ctrl Pts',(-0.24024064412003,-0.0609922781173483,
-0.990332542620729));
#13058=CARTESIAN_POINT('Ctrl Pts',(-0.236509675094874,-0.0742967091364493,
-0.991238884025248));
#13059=CARTESIAN_POINT('Ctrl Pts',(-0.221129100087819,-0.115492077056649,
-0.994830026707808));
#13060=CARTESIAN_POINT('Ctrl Pts',(-0.205111543747588,-0.141695629206859,
-0.998375294985966));
#13061=CARTESIAN_POINT('Ctrl Pts',(-0.169940289819232,-0.181890537957859,
-1.00492400591205));
#13062=CARTESIAN_POINT('Ctrl Pts',(-0.1465689792446,-0.201072148666545,
-1.00869718865384));
#13063=CARTESIAN_POINT('Ctrl Pts',(-0.106909345252087,-0.223955109275652,
-1.01358704779679));
#13064=CARTESIAN_POINT('Ctrl Pts',(-0.0861971848975942,-0.232742381310829,
-1.0156297872271));
#13065=CARTESIAN_POINT('Ctrl Pts',(-0.0430711894098823,-0.244234834628584,
-1.01837060663223));
#13066=CARTESIAN_POINT('Ctrl Pts',(-0.0206568624125606,-0.246942143572133,
-1.019052));
#13067=CARTESIAN_POINT('Ctrl Pts',(0.0206568624125607,-0.246942143572133,
-1.019052));
#13068=CARTESIAN_POINT('Ctrl Pts',(0.0430711894098824,-0.244234834628584,
-1.01837060663223));
#13069=CARTESIAN_POINT('Ctrl Pts',(0.0861971848975943,-0.232742381310829,
-1.0156297872271));
#13070=CARTESIAN_POINT('Ctrl Pts',(0.106909345252088,-0.223955109275652,
-1.01358704779679));
#13071=CARTESIAN_POINT('Ctrl Pts',(0.1465689792446,-0.201072148666545,-1.00869718865384));
#13072=CARTESIAN_POINT('Ctrl Pts',(0.169940289819232,-0.181890537957859,
-1.00492400591205));
#13073=CARTESIAN_POINT('Ctrl Pts',(0.205111543747588,-0.141695629206859,
-0.998375294985966));
#13074=CARTESIAN_POINT('Ctrl Pts',(0.221129100087819,-0.115492077056649,
-0.994830026707808));
#13075=CARTESIAN_POINT('Ctrl Pts',(0.236509675094874,-0.0742967091364493,
-0.991238884025248));
#13076=CARTESIAN_POINT('Ctrl Pts',(0.24024064412003,-0.0609922781173484,
-0.990332542620729));
#13077=CARTESIAN_POINT('Ctrl Pts',(0.242834539687907,-0.04763,-0.989696097314));
#13078=CARTESIAN_POINT('',(0.528110872004958,-0.04763,-0.871530771444223));
#13079=CARTESIAN_POINT('Origin',(0.,-0.04763,0.));
#13080=CARTESIAN_POINT('',(0.871530771444223,-0.04763,-0.528110872004958));
#13081=CARTESIAN_POINT('Ctrl Pts',(0.528110872004958,-0.0476300000000001,
-0.871530771444223));
#13082=CARTESIAN_POINT('Ctrl Pts',(0.530395067942936,-0.0609922781173484,
-0.870146645090731));
#13083=CARTESIAN_POINT('Ctrl Pts',(0.533674141594226,-0.0742967091364493,
-0.868149331745851));
#13084=CARTESIAN_POINT('Ctrl Pts',(0.54708917182331,-0.115492077056649,
-0.85981294420286));
#13085=CARTESIAN_POINT('Ctrl Pts',(0.560922177770136,-0.141695629206859,
-0.850993704737257));
#13086=CARTESIAN_POINT('Ctrl Pts',(0.590422647829571,-0.181890537957859,
-0.830754510485543));
#13087=CARTESIAN_POINT('Ctrl Pts',(0.609616703125488,-0.201072148666545,
-0.816896541396381));
#13088=CARTESIAN_POINT('Ctrl Pts',(0.641117951819998,-0.223955109275652,
-0.792310597819928));
#13089=CARTESIAN_POINT('Ctrl Pts',(0.657208095763053,-0.232742381310829,
-0.779109323683612));
#13090=CARTESIAN_POINT('Ctrl Pts',(0.68964083160521,-0.244234834628584,
-0.750552691816206));
#13091=CARTESIAN_POINT('Ctrl Pts',(0.705971972091755,-0.246942143572133,
-0.735185187071673));
#13092=CARTESIAN_POINT('Ctrl Pts',(0.735185187071673,-0.246942143572133,
-0.705971972091754));
#13093=CARTESIAN_POINT('Ctrl Pts',(0.750552691816206,-0.244234834628584,
-0.68964083160521));
#13094=CARTESIAN_POINT('Ctrl Pts',(0.779109323683612,-0.232742381310829,
-0.657208095763053));
#13095=CARTESIAN_POINT('Ctrl Pts',(0.792310597819928,-0.223955109275652,
-0.641117951819998));
#13096=CARTESIAN_POINT('Ctrl Pts',(0.816896541396381,-0.201072148666545,
-0.609616703125488));
#13097=CARTESIAN_POINT('Ctrl Pts',(0.830754510485543,-0.181890537957859,
-0.590422647829571));
#13098=CARTESIAN_POINT('Ctrl Pts',(0.850993704737257,-0.141695629206859,
-0.560922177770136));
#13099=CARTESIAN_POINT('Ctrl Pts',(0.85981294420286,-0.115492077056649,
-0.54708917182331));
#13100=CARTESIAN_POINT('Ctrl Pts',(0.868149331745851,-0.0742967091364493,
-0.533674141594226));
#13101=CARTESIAN_POINT('Ctrl Pts',(0.870146645090731,-0.0609922781173484,
-0.530395067942936));
#13102=CARTESIAN_POINT('Ctrl Pts',(0.871530771444223,-0.0476300000000001,
-0.528110872004958));
#13103=CARTESIAN_POINT('',(0.989696097314,-0.04763,-0.242834539687906));
#13104=CARTESIAN_POINT('Origin',(0.,-0.04763,0.));
#13105=CARTESIAN_POINT('',(0.989696097314,-0.04763,0.242834539687906));
#13106=CARTESIAN_POINT('Ctrl Pts',(0.989696097314,-0.04763,-0.242834539687907));
#13107=CARTESIAN_POINT('Ctrl Pts',(0.990332542620729,-0.0609922781173483,
-0.24024064412003));
#13108=CARTESIAN_POINT('Ctrl Pts',(0.991238884025248,-0.0742967091364493,
-0.236509675094874));
#13109=CARTESIAN_POINT('Ctrl Pts',(0.994830026707808,-0.115492077056649,
-0.221129100087819));
#13110=CARTESIAN_POINT('Ctrl Pts',(0.998375294985966,-0.141695629206859,
-0.205111543747588));
#13111=CARTESIAN_POINT('Ctrl Pts',(1.00492400591205,-0.181890537957859,
-0.169940289819232));
#13112=CARTESIAN_POINT('Ctrl Pts',(1.00869718865384,-0.201072148666545,
-0.1465689792446));
#13113=CARTESIAN_POINT('Ctrl Pts',(1.01358704779679,-0.223955109275652,
-0.106909345252087));
#13114=CARTESIAN_POINT('Ctrl Pts',(1.0156297872271,-0.232742381310829,-0.0861971848975942));
#13115=CARTESIAN_POINT('Ctrl Pts',(1.01837060663223,-0.244234834628584,
-0.0430711894098823));
#13116=CARTESIAN_POINT('Ctrl Pts',(1.019052,-0.246942143572133,-0.0206568624125607));
#13117=CARTESIAN_POINT('Ctrl Pts',(1.019052,-0.246942143572133,0.0206568624125607));
#13118=CARTESIAN_POINT('Ctrl Pts',(1.01837060663223,-0.244234834628584,
0.0430711894098823));
#13119=CARTESIAN_POINT('Ctrl Pts',(1.0156297872271,-0.232742381310829,0.0861971848975942));
#13120=CARTESIAN_POINT('Ctrl Pts',(1.01358704779679,-0.223955109275652,
0.106909345252087));
#13121=CARTESIAN_POINT('Ctrl Pts',(1.00869718865384,-0.201072148666545,
0.1465689792446));
#13122=CARTESIAN_POINT('Ctrl Pts',(1.00492400591205,-0.181890537957859,
0.169940289819232));
#13123=CARTESIAN_POINT('Ctrl Pts',(0.998375294985966,-0.141695629206859,
0.205111543747588));
#13124=CARTESIAN_POINT('Ctrl Pts',(0.994830026707808,-0.115492077056649,
0.221129100087819));
#13125=CARTESIAN_POINT('Ctrl Pts',(0.991238884025248,-0.0742967091364492,
0.236509675094874));
#13126=CARTESIAN_POINT('Ctrl Pts',(0.990332542620729,-0.0609922781173483,
0.24024064412003));
#13127=CARTESIAN_POINT('Ctrl Pts',(0.989696097314,-0.04763,0.242834539687907));
#13128=CARTESIAN_POINT('Origin',(0.,-0.04763,0.));
#13129=CARTESIAN_POINT('Origin',(0.,-0.04763,0.));
#13130=CARTESIAN_POINT('',(0.238183666596899,-0.04763,0.951592097314));
#13131=CARTESIAN_POINT('Origin',(0.,-0.04763,0.));
#13132=CARTESIAN_POINT('Origin',(-1.94289029309402E-16,-0.04763,1.));
#13133=CARTESIAN_POINT('Origin',(-1.94289029309402E-16,0.,1.));
#13134=CARTESIAN_POINT('',(-0.2381836665969,-0.04763,0.951592097314));
#13135=CARTESIAN_POINT('Ctrl Pts',(-0.238183666596899,-0.0476299999999999,
0.951592097314));
#13136=CARTESIAN_POINT('Ctrl Pts',(-0.233157223576062,-0.0740444353928835,
0.952850216871763));
#13137=CARTESIAN_POINT('Ctrl Pts',(-0.223801617934946,-0.0999305678883309,
0.955173119738174));
#13138=CARTESIAN_POINT('Ctrl Pts',(-0.199966927975188,-0.142345102874864,
0.960411259488514));
#13139=CARTESIAN_POINT('Ctrl Pts',(-0.1868781821531,-0.159766064500479,
0.963103647174702));
#13140=CARTESIAN_POINT('Ctrl Pts',(-0.15681442133453,-0.190326085855194,
0.968453058988463));
#13141=CARTESIAN_POINT('Ctrl Pts',(-0.139836317888043,-0.203463743702801,
0.971100730005489));
#13142=CARTESIAN_POINT('Ctrl Pts',(-0.104422493053067,-0.224161999508995,
0.975530745318961));
#13143=CARTESIAN_POINT('Ctrl Pts',(-0.0842175114474176,-0.232861760990032,
0.977553872336861));
#13144=CARTESIAN_POINT('Ctrl Pts',(-0.0421062857595701,-0.244251601209411,
0.980270995488453));
#13145=CARTESIAN_POINT('Ctrl Pts',(-0.0201990724523197,-0.246942143572133,
0.980948));
#13146=CARTESIAN_POINT('Ctrl Pts',(0.020199072452319,-0.246942143572133,
0.980948));
#13147=CARTESIAN_POINT('Ctrl Pts',(0.0421062857595694,-0.244251601209411,
0.980270995488454));
#13148=CARTESIAN_POINT('Ctrl Pts',(0.0842175114474169,-0.232861760990032,
0.977553872336861));
#13149=CARTESIAN_POINT('Ctrl Pts',(0.104422493053067,-0.224161999508995,
0.975530745318961));
#13150=CARTESIAN_POINT('Ctrl Pts',(0.139836317888042,-0.203463743702801,
0.971100730005489));
#13151=CARTESIAN_POINT('Ctrl Pts',(0.15681442133453,-0.190326085855194,
0.968453058988463));
#13152=CARTESIAN_POINT('Ctrl Pts',(0.1868781821531,-0.15976606450048,0.963103647174702));
#13153=CARTESIAN_POINT('Ctrl Pts',(0.199966927975188,-0.142345102874864,
0.960411259488514));
#13154=CARTESIAN_POINT('Ctrl Pts',(0.223801617934945,-0.0999305678883309,
0.955173119738174));
#13155=CARTESIAN_POINT('Ctrl Pts',(0.233157223576061,-0.0740444353928835,
0.952850216871763));
#13156=CARTESIAN_POINT('Ctrl Pts',(0.238183666596899,-0.0476299999999999,
0.951592097314));
#13157=CARTESIAN_POINT('Origin',(-1.94289029309402E-16,-0.04763,1.));
#13158=CARTESIAN_POINT('Origin',(0.,-0.04763,0.));
#13159=CARTESIAN_POINT('',(-0.504455939115715,-0.04763,0.841298510752802));
#13160=CARTESIAN_POINT('Origin',(0.,-0.04763,0.));
#13161=CARTESIAN_POINT('Origin',(-0.707106781186548,-0.04763,0.707106781186547));
#13162=CARTESIAN_POINT('Origin',(-0.707106781186548,0.,0.707106781186547));
#13163=CARTESIAN_POINT('',(-0.841298510752802,-0.04763,0.504455939115715));
#13164=CARTESIAN_POINT('Ctrl Pts',(-0.841298510752802,-0.04763,0.504455939115715));
#13165=CARTESIAN_POINT('Ctrl Pts',(-0.838633903678357,-0.0740444353928835,
0.508899795931835));
#13166=CARTESIAN_POINT('Ctrl Pts',(-0.833661031856294,-0.0999305678883309,
0.517157748491652));
#13167=CARTESIAN_POINT('Ctrl Pts',(-0.820511285096538,-0.142345102874864,
0.537715343527944));
#13168=CARTESIAN_POINT('Ctrl Pts',(-0.813159949759,-0.159766064500479,0.548874290046456));
#13169=CARTESIAN_POINT('Ctrl Pts',(-0.795684265985089,-0.190326085855194,
0.573915184558107));
#13170=CARTESIAN_POINT('Ctrl Pts',(-0.78555112003688,-0.203463743702801,
0.587792702767295));
#13171=CARTESIAN_POINT('Ctrl Pts',(-0.763642258217233,-0.224161999508995,
0.615966552324775));
#13172=CARTESIAN_POINT('Ctrl Pts',(-0.750785745543687,-0.232861760990032,
0.631684198665438));
#13173=CARTESIAN_POINT('Ctrl Pts',(-0.722929908501543,-0.244251601209411,
0.663382628119203));
#13174=CARTESIAN_POINT('Ctrl Pts',(-0.707917883896095,-0.246942143572133,
0.679352081686668));
#13175=CARTESIAN_POINT('Ctrl Pts',(-0.679352081686668,-0.246942143572133,
0.707917883896095));
#13176=CARTESIAN_POINT('Ctrl Pts',(-0.663382628119203,-0.244251601209411,
0.722929908501544));
#13177=CARTESIAN_POINT('Ctrl Pts',(-0.631684198665438,-0.232861760990031,
0.750785745543687));
#13178=CARTESIAN_POINT('Ctrl Pts',(-0.615966552324775,-0.224161999508995,
0.763642258217233));
#13179=CARTESIAN_POINT('Ctrl Pts',(-0.587792702767295,-0.203463743702801,
0.78555112003688));
#13180=CARTESIAN_POINT('Ctrl Pts',(-0.573915184558107,-0.190326085855194,
0.795684265985088));
#13181=CARTESIAN_POINT('Ctrl Pts',(-0.548874290046456,-0.159766064500479,
0.813159949759));
#13182=CARTESIAN_POINT('Ctrl Pts',(-0.537715343527944,-0.142345102874864,
0.820511285096538));
#13183=CARTESIAN_POINT('Ctrl Pts',(-0.517157748491652,-0.0999305678883309,
0.833661031856294));
#13184=CARTESIAN_POINT('Ctrl Pts',(-0.508899795931835,-0.0740444353928835,
0.838633903678357));
#13185=CARTESIAN_POINT('Ctrl Pts',(-0.504455939115716,-0.04763,0.841298510752801));
#13186=CARTESIAN_POINT('Origin',(-0.707106781186548,-0.04763,0.707106781186547));
#13187=CARTESIAN_POINT('Origin',(0.,-0.04763,0.));
#13188=CARTESIAN_POINT('',(-0.951592097314,-0.04763,0.238183666596899));
#13189=CARTESIAN_POINT('Origin',(0.,-0.04763,0.));
#13190=CARTESIAN_POINT('Origin',(-1.,-0.04763,-1.11022302462516E-16));
#13191=CARTESIAN_POINT('Origin',(-1.,0.,-1.11022302462516E-16));
#13192=CARTESIAN_POINT('',(-0.951592097314,-0.04763,-0.2381836665969));
#13193=CARTESIAN_POINT('',(-0.980948,-0.246942143572133,1.08514323328844E-18));
#13194=CARTESIAN_POINT('Ctrl Pts',(-0.951592097314,-0.04763,-0.238183666596899));
#13195=CARTESIAN_POINT('Ctrl Pts',(-0.952850216871763,-0.0740444353928835,
-0.233157223576062));
#13196=CARTESIAN_POINT('Ctrl Pts',(-0.955173119738174,-0.0999305678883309,
-0.223801617934946));
#13197=CARTESIAN_POINT('Ctrl Pts',(-0.960411259488514,-0.142345102874864,
-0.199966927975188));
#13198=CARTESIAN_POINT('Ctrl Pts',(-0.963103647174702,-0.159766064500479,
-0.1868781821531));
#13199=CARTESIAN_POINT('Ctrl Pts',(-0.968453058988463,-0.190326085855194,
-0.15681442133453));
#13200=CARTESIAN_POINT('Ctrl Pts',(-0.971100730005489,-0.203463743702801,
-0.139836317888043));
#13201=CARTESIAN_POINT('Ctrl Pts',(-0.975530745318961,-0.224161999508995,
-0.104422493053067));
#13202=CARTESIAN_POINT('Ctrl Pts',(-0.977553872336861,-0.232861760990032,
-0.0842175114474175));
#13203=CARTESIAN_POINT('Ctrl Pts',(-0.980270995488453,-0.244251601209411,
-0.0421062857595699));
#13204=CARTESIAN_POINT('Ctrl Pts',(-0.980948,-0.246942143572133,-0.0201990724523195));
#13205=CARTESIAN_POINT('Ctrl Pts',(-0.980948,-0.246942143572133,-1.17961196366423E-16));
#13206=CARTESIAN_POINT('Origin',(-1.,-0.04763,-1.11022302462516E-16));
#13207=CARTESIAN_POINT('Ctrl Pts',(-0.980948,-0.246942143572133,-1.17961196366423E-16));
#13208=CARTESIAN_POINT('Ctrl Pts',(-0.980948,-0.246942143572133,0.0201990724523192));
#13209=CARTESIAN_POINT('Ctrl Pts',(-0.980270995488453,-0.244251601209411,
0.0421062857595695));
#13210=CARTESIAN_POINT('Ctrl Pts',(-0.977553872336861,-0.232861760990032,
0.0842175114474169));
#13211=CARTESIAN_POINT('Ctrl Pts',(-0.975530745318961,-0.224161999508995,
0.104422493053066));
#13212=CARTESIAN_POINT('Ctrl Pts',(-0.971100730005489,-0.203463743702801,
0.139836317888042));
#13213=CARTESIAN_POINT('Ctrl Pts',(-0.968453058988463,-0.190326085855194,
0.15681442133453));
#13214=CARTESIAN_POINT('Ctrl Pts',(-0.963103647174702,-0.15976606450048,
0.1868781821531));
#13215=CARTESIAN_POINT('Ctrl Pts',(-0.960411259488514,-0.142345102874864,
0.199966927975188));
#13216=CARTESIAN_POINT('Ctrl Pts',(-0.955173119738174,-0.099930567888331,
0.223801617934945));
#13217=CARTESIAN_POINT('Ctrl Pts',(-0.952850216871763,-0.0740444353928835,
0.233157223576061));
#13218=CARTESIAN_POINT('Ctrl Pts',(-0.951592097314,-0.04763,0.238183666596899));
#13219=CARTESIAN_POINT('Origin',(0.,-0.04763,0.));
#13220=CARTESIAN_POINT('',(-0.841298510752802,-0.04763,-0.504455939115715));
#13221=CARTESIAN_POINT('Origin',(0.,-0.04763,0.));
#13222=CARTESIAN_POINT('Origin',(-0.707106781186547,-0.04763,-0.707106781186548));
#13223=CARTESIAN_POINT('Origin',(-0.707106781186547,0.,-0.707106781186548));
#13224=CARTESIAN_POINT('',(-0.504455939115715,-0.04763,-0.841298510752802));
#13225=CARTESIAN_POINT('Ctrl Pts',(-0.504455939115715,-0.04763,-0.841298510752802));
#13226=CARTESIAN_POINT('Ctrl Pts',(-0.508899795931835,-0.0740444353928835,
-0.838633903678357));
#13227=CARTESIAN_POINT('Ctrl Pts',(-0.517157748491652,-0.0999305678883309,
-0.833661031856294));
#13228=CARTESIAN_POINT('Ctrl Pts',(-0.537715343527944,-0.142345102874864,
-0.820511285096538));
#13229=CARTESIAN_POINT('Ctrl Pts',(-0.548874290046456,-0.159766064500479,
-0.813159949759));
#13230=CARTESIAN_POINT('Ctrl Pts',(-0.573915184558107,-0.190326085855194,
-0.795684265985089));
#13231=CARTESIAN_POINT('Ctrl Pts',(-0.587792702767295,-0.203463743702801,
-0.78555112003688));
#13232=CARTESIAN_POINT('Ctrl Pts',(-0.615966552324775,-0.224161999508995,
-0.763642258217233));
#13233=CARTESIAN_POINT('Ctrl Pts',(-0.631684198665438,-0.232861760990032,
-0.750785745543687));
#13234=CARTESIAN_POINT('Ctrl Pts',(-0.663382628119203,-0.244251601209411,
-0.722929908501543));
#13235=CARTESIAN_POINT('Ctrl Pts',(-0.679352081686668,-0.246942143572133,
-0.707917883896095));
#13236=CARTESIAN_POINT('Ctrl Pts',(-0.707917883896095,-0.246942143572133,
-0.679352081686668));
#13237=CARTESIAN_POINT('Ctrl Pts',(-0.722929908501543,-0.244251601209411,
-0.663382628119203));
#13238=CARTESIAN_POINT('Ctrl Pts',(-0.750785745543687,-0.232861760990032,
-0.631684198665439));
#13239=CARTESIAN_POINT('Ctrl Pts',(-0.763642258217232,-0.224161999508995,
-0.615966552324775));
#13240=CARTESIAN_POINT('Ctrl Pts',(-0.78555112003688,-0.203463743702801,
-0.587792702767295));
#13241=CARTESIAN_POINT('Ctrl Pts',(-0.795684265985088,-0.190326085855194,
-0.573915184558107));
#13242=CARTESIAN_POINT('Ctrl Pts',(-0.813159949759,-0.15976606450048,-0.548874290046456));
#13243=CARTESIAN_POINT('Ctrl Pts',(-0.820511285096538,-0.142345102874864,
-0.537715343527944));
#13244=CARTESIAN_POINT('Ctrl Pts',(-0.833661031856294,-0.0999305678883311,
-0.517157748491652));
#13245=CARTESIAN_POINT('Ctrl Pts',(-0.838633903678357,-0.0740444353928836,
-0.508899795931835));
#13246=CARTESIAN_POINT('Ctrl Pts',(-0.841298510752801,-0.04763,-0.504455939115715));
#13247=CARTESIAN_POINT('Origin',(-0.707106781186547,-0.04763,-0.707106781186548));
#13248=CARTESIAN_POINT('Origin',(0.,-0.04763,0.));
#13249=CARTESIAN_POINT('',(-0.238183666596899,-0.04763,-0.951592097314));
#13250=CARTESIAN_POINT('Origin',(0.,-0.04763,0.));
#13251=CARTESIAN_POINT('Origin',(5.55111512312578E-17,-0.04763,-1.));
#13252=CARTESIAN_POINT('Origin',(5.55111512312578E-17,0.,-1.));
#13253=CARTESIAN_POINT('',(0.238183666596899,-0.04763,-0.951592097314));
#13254=CARTESIAN_POINT('Ctrl Pts',(0.238183666596899,-0.04763,-0.951592097314));
#13255=CARTESIAN_POINT('Ctrl Pts',(0.233157223576062,-0.0740444353928835,
-0.952850216871763));
#13256=CARTESIAN_POINT('Ctrl Pts',(0.223801617934946,-0.099930567888331,
-0.955173119738174));
#13257=CARTESIAN_POINT('Ctrl Pts',(0.199966927975188,-0.142345102874864,
-0.960411259488514));
#13258=CARTESIAN_POINT('Ctrl Pts',(0.1868781821531,-0.15976606450048,-0.963103647174702));
#13259=CARTESIAN_POINT('Ctrl Pts',(0.15681442133453,-0.190326085855194,
-0.968453058988463));
#13260=CARTESIAN_POINT('Ctrl Pts',(0.139836317888042,-0.203463743702801,
-0.971100730005489));
#13261=CARTESIAN_POINT('Ctrl Pts',(0.104422493053067,-0.224161999508995,
-0.975530745318961));
#13262=CARTESIAN_POINT('Ctrl Pts',(0.0842175114474173,-0.232861760990032,
-0.977553872336861));
#13263=CARTESIAN_POINT('Ctrl Pts',(0.0421062857595698,-0.244251601209411,
-0.980270995488453));
#13264=CARTESIAN_POINT('Ctrl Pts',(0.0201990724523194,-0.246942143572133,
-0.980948));
#13265=CARTESIAN_POINT('Ctrl Pts',(-0.0201990724523193,-0.246942143572133,
-0.980948));
#13266=CARTESIAN_POINT('Ctrl Pts',(-0.0421062857595697,-0.244251601209411,
-0.980270995488453));
#13267=CARTESIAN_POINT('Ctrl Pts',(-0.0842175114474171,-0.232861760990032,
-0.977553872336861));
#13268=CARTESIAN_POINT('Ctrl Pts',(-0.104422493053067,-0.224161999508995,
-0.975530745318961));
#13269=CARTESIAN_POINT('Ctrl Pts',(-0.139836317888042,-0.203463743702801,
-0.971100730005489));
#13270=CARTESIAN_POINT('Ctrl Pts',(-0.15681442133453,-0.190326085855194,
-0.968453058988463));
#13271=CARTESIAN_POINT('Ctrl Pts',(-0.1868781821531,-0.15976606450048,-0.963103647174702));
#13272=CARTESIAN_POINT('Ctrl Pts',(-0.199966927975188,-0.142345102874864,
-0.960411259488514));
#13273=CARTESIAN_POINT('Ctrl Pts',(-0.223801617934945,-0.099930567888331,
-0.955173119738174));
#13274=CARTESIAN_POINT('Ctrl Pts',(-0.233157223576062,-0.0740444353928835,
-0.952850216871763));
#13275=CARTESIAN_POINT('Ctrl Pts',(-0.238183666596899,-0.0476299999999999,
-0.951592097314));
#13276=CARTESIAN_POINT('Origin',(5.55111512312578E-17,-0.04763,-1.));
#13277=CARTESIAN_POINT('Origin',(0.,-0.04763,0.));
#13278=CARTESIAN_POINT('',(0.504455939115715,-0.04763,-0.841298510752802));
#13279=CARTESIAN_POINT('Origin',(0.,-0.04763,0.));
#13280=CARTESIAN_POINT('Origin',(0.707106781186548,-0.04763,-0.707106781186547));
#13281=CARTESIAN_POINT('Origin',(0.707106781186548,0.,-0.707106781186547));
#13282=CARTESIAN_POINT('',(0.841298510752802,-0.04763,-0.504455939115715));
#13283=CARTESIAN_POINT('Ctrl Pts',(0.841298510752802,-0.04763,-0.504455939115715));
#13284=CARTESIAN_POINT('Ctrl Pts',(0.838633903678357,-0.0740444353928835,
-0.508899795931835));
#13285=CARTESIAN_POINT('Ctrl Pts',(0.833661031856294,-0.0999305678883309,
-0.517157748491652));
#13286=CARTESIAN_POINT('Ctrl Pts',(0.820511285096538,-0.142345102874864,
-0.537715343527944));
#13287=CARTESIAN_POINT('Ctrl Pts',(0.813159949759,-0.159766064500479,-0.548874290046456));
#13288=CARTESIAN_POINT('Ctrl Pts',(0.795684265985088,-0.190326085855194,
-0.573915184558107));
#13289=CARTESIAN_POINT('Ctrl Pts',(0.78555112003688,-0.203463743702801,
-0.587792702767295));
#13290=CARTESIAN_POINT('Ctrl Pts',(0.763642258217233,-0.224161999508995,
-0.615966552324775));
#13291=CARTESIAN_POINT('Ctrl Pts',(0.750785745543687,-0.232861760990032,
-0.631684198665438));
#13292=CARTESIAN_POINT('Ctrl Pts',(0.722929908501543,-0.244251601209411,
-0.663382628119203));
#13293=CARTESIAN_POINT('Ctrl Pts',(0.707917883896095,-0.246942143572133,
-0.679352081686668));
#13294=CARTESIAN_POINT('Ctrl Pts',(0.679352081686668,-0.246942143572133,
-0.707917883896095));
#13295=CARTESIAN_POINT('Ctrl Pts',(0.663382628119203,-0.244251601209411,
-0.722929908501543));
#13296=CARTESIAN_POINT('Ctrl Pts',(0.631684198665438,-0.232861760990032,
-0.750785745543687));
#13297=CARTESIAN_POINT('Ctrl Pts',(0.615966552324775,-0.224161999508995,
-0.763642258217232));
#13298=CARTESIAN_POINT('Ctrl Pts',(0.587792702767295,-0.203463743702801,
-0.78555112003688));
#13299=CARTESIAN_POINT('Ctrl Pts',(0.573915184558107,-0.190326085855194,
-0.795684265985088));
#13300=CARTESIAN_POINT('Ctrl Pts',(0.548874290046456,-0.159766064500479,
-0.813159949759));
#13301=CARTESIAN_POINT('Ctrl Pts',(0.537715343527944,-0.142345102874864,
-0.820511285096538));
#13302=CARTESIAN_POINT('Ctrl Pts',(0.517157748491652,-0.099930567888331,
-0.833661031856294));
#13303=CARTESIAN_POINT('Ctrl Pts',(0.508899795931835,-0.0740444353928835,
-0.838633903678357));
#13304=CARTESIAN_POINT('Ctrl Pts',(0.504455939115715,-0.04763,-0.841298510752801));
#13305=CARTESIAN_POINT('Origin',(0.707106781186548,-0.04763,-0.707106781186547));
#13306=CARTESIAN_POINT('Origin',(0.,-0.166705,0.));
#13307=CARTESIAN_POINT('',(-0.980948,-0.28578,1.20131482833E-16));
#13308=CARTESIAN_POINT('Origin',(0.,-0.28578,0.));
#13309=CARTESIAN_POINT('',(-0.980948,-0.166705,1.20131482833E-16));
#13310=CARTESIAN_POINT('',(0.951592097314,-0.04763,0.238183666596899));
#13311=CARTESIAN_POINT('Origin',(0.,-0.04763,0.));
#13312=CARTESIAN_POINT('',(0.951592097314,-0.04763,-0.238183666596899));
#13313=CARTESIAN_POINT('Ctrl Pts',(0.951592097314,-0.04763,0.238183666596899));
#13314=CARTESIAN_POINT('Ctrl Pts',(0.952850216871763,-0.0740444353928835,
0.233157223576062));
#13315=CARTESIAN_POINT('Ctrl Pts',(0.955173119738174,-0.099930567888331,
0.223801617934945));
#13316=CARTESIAN_POINT('Ctrl Pts',(0.960411259488514,-0.142345102874864,
0.199966927975188));
#13317=CARTESIAN_POINT('Ctrl Pts',(0.963103647174702,-0.15976606450048,
0.1868781821531));
#13318=CARTESIAN_POINT('Ctrl Pts',(0.968453058988463,-0.190326085855194,
0.15681442133453));
#13319=CARTESIAN_POINT('Ctrl Pts',(0.971100730005489,-0.203463743702801,
0.139836317888042));
#13320=CARTESIAN_POINT('Ctrl Pts',(0.975530745318961,-0.224161999508995,
0.104422493053067));
#13321=CARTESIAN_POINT('Ctrl Pts',(0.977553872336861,-0.232861760990032,
0.0842175114474172));
#13322=CARTESIAN_POINT('Ctrl Pts',(0.980270995488453,-0.244251601209411,
0.0421062857595697));
#13323=CARTESIAN_POINT('Ctrl Pts',(0.980948,-0.246942143572133,0.0201990724523194));
#13324=CARTESIAN_POINT('Ctrl Pts',(0.980948,-0.246942143572133,-0.0201990724523194));
#13325=CARTESIAN_POINT('Ctrl Pts',(0.980270995488453,-0.244251601209411,
-0.0421062857595697));
#13326=CARTESIAN_POINT('Ctrl Pts',(0.977553872336861,-0.232861760990032,
-0.0842175114474172));
#13327=CARTESIAN_POINT('Ctrl Pts',(0.975530745318961,-0.224161999508995,
-0.104422493053067));
#13328=CARTESIAN_POINT('Ctrl Pts',(0.971100730005489,-0.203463743702801,
-0.139836317888042));
#13329=CARTESIAN_POINT('Ctrl Pts',(0.968453058988463,-0.190326085855194,
-0.15681442133453));
#13330=CARTESIAN_POINT('Ctrl Pts',(0.963103647174702,-0.15976606450048,
-0.1868781821531));
#13331=CARTESIAN_POINT('Ctrl Pts',(0.960411259488514,-0.142345102874864,
-0.199966927975188));
#13332=CARTESIAN_POINT('Ctrl Pts',(0.955173119738174,-0.099930567888331,
-0.223801617934945));
#13333=CARTESIAN_POINT('Ctrl Pts',(0.952850216871763,-0.0740444353928835,
-0.233157223576062));
#13334=CARTESIAN_POINT('Ctrl Pts',(0.951592097314,-0.0476299999999999,-0.238183666596899));
#13335=CARTESIAN_POINT('Origin',(0.,-0.04763,0.));
#13336=CARTESIAN_POINT('Origin',(0.,-0.04763,0.));
#13337=CARTESIAN_POINT('Origin',(1.,-0.04763,0.));
#13338=CARTESIAN_POINT('Origin',(1.,0.,0.));
#13339=CARTESIAN_POINT('Origin',(1.,-0.04763,0.));
#13340=CARTESIAN_POINT('Origin',(0.,-0.28578,0.));
#13341=CARTESIAN_POINT('Origin',(0.,-0.04763,0.));
#13342=CARTESIAN_POINT('',(0.,0.,0.));
#13343=CARTESIAN_POINT('Origin',(1.013815,0.445,0.));
#13344=CARTESIAN_POINT('',(-1.013815,0.445,-1.24156529467757E-16));
#13345=CARTESIAN_POINT('Origin',(0.,0.445,0.));
#13346=CARTESIAN_POINT('',(-0.991185,0.445,-1.21385153761287E-16));
#13347=CARTESIAN_POINT('Origin',(0.,0.445,0.));
#13348=CARTESIAN_POINT('Origin',(0.,0.4075,0.));
#13349=CARTESIAN_POINT('',(-1.013815,0.37,-1.24156529467757E-16));
#13350=CARTESIAN_POINT('Origin',(0.,0.37,0.));
#13351=CARTESIAN_POINT('',(-1.013815,0.4075,-1.24156529467757E-16));
#13352=CARTESIAN_POINT('Origin',(0.991185,0.37,0.));
#13353=CARTESIAN_POINT('',(-0.991185,0.37,-1.21385153761287E-16));
#13354=CARTESIAN_POINT('Origin',(0.,0.37,0.));
#13355=CARTESIAN_POINT('Origin',(0.,0.4075,0.));
#13356=CARTESIAN_POINT('',(-0.991185,0.4075,-1.21385153761287E-16));
#13357=CARTESIAN_POINT('Origin',(1.013815,-0.37,0.));
#13358=CARTESIAN_POINT('',(-1.013815,-0.37,-1.24156529467757E-16));
#13359=CARTESIAN_POINT('Origin',(0.,-0.37,0.));
#13360=CARTESIAN_POINT('',(-0.991185,-0.37,-1.21385153761287E-16));
#13361=CARTESIAN_POINT('Origin',(0.,-0.37,0.));
#13362=CARTESIAN_POINT('Origin',(0.,-0.4075,0.));
#13363=CARTESIAN_POINT('',(-1.013815,-0.445,-1.24156529467757E-16));
#13364=CARTESIAN_POINT('Origin',(0.,-0.445,0.));
#13365=CARTESIAN_POINT('',(-1.013815,-0.4075,-1.24156529467757E-16));
#13366=CARTESIAN_POINT('Origin',(0.991185,-0.445,0.));
#13367=CARTESIAN_POINT('',(-0.991185,-0.445,-1.21385153761287E-16));
#13368=CARTESIAN_POINT('Origin',(0.,-0.445,0.));
#13369=CARTESIAN_POINT('Origin',(0.,-0.4075,0.));
#13370=CARTESIAN_POINT('',(-0.991185,-0.4075,-1.21385153761287E-16));
#13371=CARTESIAN_POINT('',(0.,0.,0.));
#13372=CARTESIAN_POINT('',(0.,0.,0.));
#13373=CARTESIAN_POINT('',(0.,0.,0.));
#13374=CARTESIAN_POINT('',(0.,0.,0.));
#13375=CARTESIAN_POINT('',(0.,0.,0.));
#13376=CARTESIAN_POINT('',(0.,0.,0.));
#13377=CARTESIAN_POINT('',(0.,0.,0.));
#13378=CARTESIAN_POINT('Origin',(-3.2,6.,4.7));
#13379=CARTESIAN_POINT('',(-3.425,6.,4.8));
#13380=CARTESIAN_POINT('Origin',(-3.2,6.,4.8));
#13381=CARTESIAN_POINT('',(-3.425,6.,5.6));
#13382=CARTESIAN_POINT('',(-3.425,6.,4.7));
#13383=CARTESIAN_POINT('Origin',(-3.2,6.,5.6));
#13384=CARTESIAN_POINT('Origin',(-3.2,6.,4.8));
#13385=CARTESIAN_POINT('',(-2.71010205144336,5.5,5.6));
#13386=CARTESIAN_POINT('',(-2.71010205144336,5.5,4.8));
#13387=CARTESIAN_POINT('',(-2.71010205144336,5.5,4.8));
#13388=CARTESIAN_POINT('',(-2.71010205144336,6.5,5.6));
#13389=CARTESIAN_POINT('Origin',(-3.2,6.,5.6));
#13390=CARTESIAN_POINT('',(-2.71010205144336,6.5,4.8));
#13391=CARTESIAN_POINT('',(-2.71010205144336,6.5,4.8));
#13392=CARTESIAN_POINT('Origin',(-3.2,6.,4.8));
#13393=CARTESIAN_POINT('Origin',(-3.2,5.5,4.8));
#13394=CARTESIAN_POINT('',(-1.09087121146357,5.5,4.8));
#13395=CARTESIAN_POINT('',(0.,5.5,4.8));
#13396=CARTESIAN_POINT('',(-1.09087121146357,5.5,5.6));
#13397=CARTESIAN_POINT('',(-1.09087121146357,5.5,4.8));
#13398=CARTESIAN_POINT('',(0.,5.5,5.6));
#13399=CARTESIAN_POINT('Origin',(0.,6.,4.8));
#13400=CARTESIAN_POINT('',(-1.09087121146357,6.5,4.8));
#13401=CARTESIAN_POINT('',(-3.2,6.5,4.8));
#13402=CARTESIAN_POINT('',(-0.5,7.09087121146357,4.8));
#13403=CARTESIAN_POINT('Origin',(0.,6.,4.8));
#13404=CARTESIAN_POINT('',(-0.5,8.51010205144336,4.8));
#13405=CARTESIAN_POINT('',(-0.5,6.,4.8));
#13406=CARTESIAN_POINT('',(0.5,8.51010205144336,4.8));
#13407=CARTESIAN_POINT('Origin',(0.,9.,4.8));
#13408=CARTESIAN_POINT('',(0.5,7.09087121146357,4.8));
#13409=CARTESIAN_POINT('',(0.5,9.,4.8));
#13410=CARTESIAN_POINT('Origin',(0.,6.,4.8));
#13411=CARTESIAN_POINT('',(-0.25,9.,4.8));
#13412=CARTESIAN_POINT('Origin',(0.,9.,4.8));
#13413=CARTESIAN_POINT('',(-0.7,6.,4.8));
#13414=CARTESIAN_POINT('Origin',(0.,6.,4.8));
#13415=CARTESIAN_POINT('Origin',(0.,6.5,4.8));
#13416=CARTESIAN_POINT('',(-1.09087121146357,6.5,5.6));
#13417=CARTESIAN_POINT('',(-3.2,6.5,5.6));
#13418=CARTESIAN_POINT('',(-1.09087121146357,6.5,4.8));
#13419=CARTESIAN_POINT('Origin',(0.,6.,4.8));
#13420=CARTESIAN_POINT('',(-0.5,7.09087121146357,5.6));
#13421=CARTESIAN_POINT('Origin',(0.,6.,5.6));
#13422=CARTESIAN_POINT('',(-0.5,7.09087121146357,4.8));
#13423=CARTESIAN_POINT('Origin',(0.,9.,4.7));
#13424=CARTESIAN_POINT('',(-0.25,9.,5.6));
#13425=CARTESIAN_POINT('',(-0.25,9.,4.7));
#13426=CARTESIAN_POINT('Origin',(0.,9.,5.6));
#13427=CARTESIAN_POINT('Origin',(0.,9.,4.8));
#13428=CARTESIAN_POINT('',(0.5,8.51010205144336,5.6));
#13429=CARTESIAN_POINT('',(0.5,8.51010205144336,4.8));
#13430=CARTESIAN_POINT('',(-0.5,8.51010205144336,5.6));
#13431=CARTESIAN_POINT('',(-0.5,8.51010205144336,4.8));
#13432=CARTESIAN_POINT('Origin',(0.,9.,5.6));
#13433=CARTESIAN_POINT('Origin',(0.5,6.,4.8));
#13434=CARTESIAN_POINT('',(0.5,7.09087121146357,5.6));
#13435=CARTESIAN_POINT('',(0.5,9.,5.6));
#13436=CARTESIAN_POINT('',(0.5,7.09087121146357,4.8));
#13437=CARTESIAN_POINT('Origin',(0.,6.,5.6));
#13438=CARTESIAN_POINT('Origin',(0.,6.,5.6));
#13439=CARTESIAN_POINT('',(-0.5,6.,5.6));
#13440=CARTESIAN_POINT('Origin',(-0.5,9.,4.8));
#13441=CARTESIAN_POINT('Origin',(0.,6.,4.8));
#13442=CARTESIAN_POINT('Origin',(0.,6.,2.95));
#13443=CARTESIAN_POINT('',(-0.7,6.,2.95));
#13444=CARTESIAN_POINT('Origin',(0.,6.,2.95));
#13445=CARTESIAN_POINT('',(-0.5,6.,2.95));
#13446=CARTESIAN_POINT('Origin',(0.,6.,2.95));
#13447=CARTESIAN_POINT('Origin',(0.,6.,2.95));
#13448=CARTESIAN_POINT('',(-0.7,6.,2.95));
#13449=CARTESIAN_POINT('Origin',(0.,6.,1.));
#13450=CARTESIAN_POINT('',(-0.5,6.,1.));
#13451=CARTESIAN_POINT('',(-0.5,6.,1.));
#13452=CARTESIAN_POINT('Origin',(0.,6.,1.));
#13453=CARTESIAN_POINT('Origin',(0.,6.,1.));
#13454=CARTESIAN_POINT('',(0.,0.,0.));
#13455=CARTESIAN_POINT('Origin',(-3.2,6.,3.9));
#13456=CARTESIAN_POINT('',(-3.365,6.,3.9));
#13457=CARTESIAN_POINT('Origin',(-3.2,6.,3.9));
#13458=CARTESIAN_POINT('',(-3.365,6.,4.8));
#13459=CARTESIAN_POINT('',(-3.365,6.,3.9));
#13460=CARTESIAN_POINT('Origin',(-3.2,6.,4.8));
#13461=CARTESIAN_POINT('Origin',(-3.2,6.,3.9));
#13462=CARTESIAN_POINT('Origin',(-3.2,6.,2.4));
#13463=CARTESIAN_POINT('',(-3.8,6.,4.8));
#13464=CARTESIAN_POINT('Origin',(-3.2,6.,4.8));
#13465=CARTESIAN_POINT('',(-3.8,6.,2.4));
#13466=CARTESIAN_POINT('',(-3.8,6.,2.4));
#13467=CARTESIAN_POINT('Origin',(-3.2,6.,2.4));
#13468=CARTESIAN_POINT('Origin',(-3.2,6.,4.8));
#13469=CARTESIAN_POINT('Origin',(-3.2,6.,2.4));
#13470=CARTESIAN_POINT('',(0.,0.,0.));
#13471=CARTESIAN_POINT('Origin',(0.,6.,1.8));
#13472=CARTESIAN_POINT('',(-0.505,6.,2.05));
#13473=CARTESIAN_POINT('Origin',(0.,6.,2.05));
#13474=CARTESIAN_POINT('',(-0.505,6.,1.8));
#13475=CARTESIAN_POINT('',(-0.505,6.,1.8));
#13476=CARTESIAN_POINT('Origin',(0.,6.,1.8));
#13477=CARTESIAN_POINT('Origin',(0.,6.,1.8));
#13478=CARTESIAN_POINT('',(-0.7,6.,2.05));
#13479=CARTESIAN_POINT('Origin',(0.,6.,2.05));
#13480=CARTESIAN_POINT('',(-0.7,6.,1.8));
#13481=CARTESIAN_POINT('',(-0.7,6.,1.8));
#13482=CARTESIAN_POINT('Origin',(0.,6.,1.8));
#13483=CARTESIAN_POINT('Origin',(0.,6.,2.05));
#13484=CARTESIAN_POINT('Origin',(0.,6.,1.8));
#13485=CARTESIAN_POINT('',(0.,0.,0.));
#13486=CARTESIAN_POINT('Origin',(0.49,6.,1.4));
#13487=CARTESIAN_POINT('',(0.49,6.12216791722871,1.28909463493591));
#13488=CARTESIAN_POINT('',(0.49,6.12216791722871,1.51090536506409));
#13489=CARTESIAN_POINT('',(0.49,6.12216791722871,1.));
#13490=CARTESIAN_POINT('Origin',(0.49,6.,1.4));
#13491=CARTESIAN_POINT('Origin',(0.49,6.,1.4));
#13492=CARTESIAN_POINT('',(0.49,5.87783208277129,1.28909463493591));
#13493=CARTESIAN_POINT('Ctrl Pts',(0.49,5.87783208277129,1.28909463493591));
#13494=CARTESIAN_POINT('Ctrl Pts',(0.490448531679987,5.8796310863737,1.28711294069536));
#13495=CARTESIAN_POINT('Ctrl Pts',(0.490895245371684,5.88146510343477,1.28518965877367));
#13496=CARTESIAN_POINT('Ctrl Pts',(0.494795015531646,5.89788800698064,1.2687667552278));
#13497=CARTESIAN_POINT('Ctrl Pts',(0.498442514607594,5.91634028497757,1.25609154388858));
#13498=CARTESIAN_POINT('Ctrl Pts',(0.50357781976106,5.95695040395284,1.23920409039234));
#13499=CARTESIAN_POINT('Ctrl Pts',(0.505,5.97911990566926,1.235));
#13500=CARTESIAN_POINT('Ctrl Pts',(0.505,6.02088009433074,1.235));
#13501=CARTESIAN_POINT('Ctrl Pts',(0.50357781976106,6.04304959604716,1.23920409039234));
#13502=CARTESIAN_POINT('Ctrl Pts',(0.498442514607594,6.08365971502243,1.25609154388858));
#13503=CARTESIAN_POINT('Ctrl Pts',(0.494795015531646,6.10211199301936,1.2687667552278));
#13504=CARTESIAN_POINT('Ctrl Pts',(0.490895245371684,6.11853489656523,1.28518965877367));
#13505=CARTESIAN_POINT('Ctrl Pts',(0.490448531679987,6.1203689136263,1.28711294069536));
#13506=CARTESIAN_POINT('Ctrl Pts',(0.49,6.12216791722871,1.28909463493591));
#13507=CARTESIAN_POINT('',(0.49,5.87783208277129,1.51090536506409));
#13508=CARTESIAN_POINT('Origin',(0.49,6.,1.4));
#13509=CARTESIAN_POINT('',(0.505,6.,1.565));
#13510=CARTESIAN_POINT('Ctrl Pts',(0.505,6.,1.565));
#13511=CARTESIAN_POINT('Ctrl Pts',(0.505,5.97911990566926,1.565));
#13512=CARTESIAN_POINT('Ctrl Pts',(0.50357781976106,5.95695040395284,1.56079590960766));
#13513=CARTESIAN_POINT('Ctrl Pts',(0.498442514607594,5.91634028497757,1.54390845611142));
#13514=CARTESIAN_POINT('Ctrl Pts',(0.494795015531646,5.89788800698064,1.5312332447722));
#13515=CARTESIAN_POINT('Ctrl Pts',(0.490895245371684,5.88146510343477,1.51481034122633));
#13516=CARTESIAN_POINT('Ctrl Pts',(0.490448531679987,5.8796310863737,1.51288705930464));
#13517=CARTESIAN_POINT('Ctrl Pts',(0.49,5.87783208277129,1.51090536506409));
#13518=CARTESIAN_POINT('',(0.9,6.,1.565));
#13519=CARTESIAN_POINT('',(0.49,6.,1.565));
#13520=CARTESIAN_POINT('',(0.884745726183518,6.165,1.4));
#13521=CARTESIAN_POINT('Ctrl Pts',(0.884745726183518,6.165,1.4));
#13522=CARTESIAN_POINT('Ctrl Pts',(0.884745726183518,6.165,1.37923124059256));
#13523=CARTESIAN_POINT('Ctrl Pts',(0.885552759505264,6.16083971900758,1.35711110492666));
#13524=CARTESIAN_POINT('Ctrl Pts',(0.888448648150043,6.14398647021669,1.31647293736623));
#13525=CARTESIAN_POINT('Ctrl Pts',(0.890493604851638,6.13129599381419,1.29795075602263));
#13526=CARTESIAN_POINT('Ctrl Pts',(0.89431723432394,6.10204981900812,1.26870458121656));
#13527=CARTESIAN_POINT('Ctrl Pts',(0.896347088899543,6.08352739209068,1.25601365401642));
#13528=CARTESIAN_POINT('Ctrl Pts',(0.899208271860583,6.04288837609341,1.23916007816136));
#13529=CARTESIAN_POINT('Ctrl Pts',(0.9,6.02076794272351,1.235));
#13530=CARTESIAN_POINT('Ctrl Pts',(0.9,5.97923205727649,1.235));
#13531=CARTESIAN_POINT('Ctrl Pts',(0.899208271860583,5.95711162390659,1.23916007816136));
#13532=CARTESIAN_POINT('Ctrl Pts',(0.896347088899543,5.91647260790932,1.25601365401642));
#13533=CARTESIAN_POINT('Ctrl Pts',(0.89431723432394,5.89795018099188,1.26870458121656));
#13534=CARTESIAN_POINT('Ctrl Pts',(0.890493604851638,5.86870400618581,1.29795075602263));
#13535=CARTESIAN_POINT('Ctrl Pts',(0.888448648150043,5.85601352978331,1.31647293736623));
#13536=CARTESIAN_POINT('Ctrl Pts',(0.885552759505264,5.83916028099242,1.35711110492666));
#13537=CARTESIAN_POINT('Ctrl Pts',(0.884745726183518,5.835,1.37923124059256));
#13538=CARTESIAN_POINT('Ctrl Pts',(0.884745726183518,5.835,1.42076875940744));
#13539=CARTESIAN_POINT('Ctrl Pts',(0.885552759505264,5.83916028099242,1.44288889507334));
#13540=CARTESIAN_POINT('Ctrl Pts',(0.888448648150043,5.85601352978331,1.48352706263377));
#13541=CARTESIAN_POINT('Ctrl Pts',(0.890493604851638,5.86870400618581,1.50204924397737));
#13542=CARTESIAN_POINT('Ctrl Pts',(0.89431723432394,5.89795018099188,1.53129541878344));
#13543=CARTESIAN_POINT('Ctrl Pts',(0.896347088899543,5.91647260790932,1.54398634598358));
#13544=CARTESIAN_POINT('Ctrl Pts',(0.899208271860583,5.95711162390659,1.56083992183864));
#13545=CARTESIAN_POINT('Ctrl Pts',(0.9,5.97923205727649,1.565));
#13546=CARTESIAN_POINT('Ctrl Pts',(0.9,6.,1.565));
#13547=CARTESIAN_POINT('Ctrl Pts',(0.9,6.,1.565));
#13548=CARTESIAN_POINT('Ctrl Pts',(0.9,6.02076794272351,1.565));
#13549=CARTESIAN_POINT('Ctrl Pts',(0.899208271860583,6.04288837609341,1.56083992183864));
#13550=CARTESIAN_POINT('Ctrl Pts',(0.896347088899543,6.08352739209068,1.54398634598358));
#13551=CARTESIAN_POINT('Ctrl Pts',(0.89431723432394,6.10204981900812,1.53129541878344));
#13552=CARTESIAN_POINT('Ctrl Pts',(0.890493604851638,6.13129599381419,1.50204924397737));
#13553=CARTESIAN_POINT('Ctrl Pts',(0.888448648150043,6.14398647021669,1.48352706263377));
#13554=CARTESIAN_POINT('Ctrl Pts',(0.885552759505264,6.16083971900758,1.44288889507334));
#13555=CARTESIAN_POINT('Ctrl Pts',(0.884745726183518,6.165,1.42076875940744));
#13556=CARTESIAN_POINT('Ctrl Pts',(0.884745726183518,6.165,1.4));
#13557=CARTESIAN_POINT('Ctrl Pts',(0.49,6.12216791722871,1.51090536506409));
#13558=CARTESIAN_POINT('Ctrl Pts',(0.490448531679987,6.1203689136263,1.51288705930464));
#13559=CARTESIAN_POINT('Ctrl Pts',(0.490895245371684,6.11853489656523,1.51481034122633));
#13560=CARTESIAN_POINT('Ctrl Pts',(0.494795015531646,6.10211199301936,1.5312332447722));
#13561=CARTESIAN_POINT('Ctrl Pts',(0.498442514607594,6.08365971502243,1.54390845611142));
#13562=CARTESIAN_POINT('Ctrl Pts',(0.50357781976106,6.04304959604716,1.56079590960766));
#13563=CARTESIAN_POINT('Ctrl Pts',(0.505,6.02088009433074,1.565));
#13564=CARTESIAN_POINT('Ctrl Pts',(0.505,6.,1.565));
#13565=CARTESIAN_POINT('Origin',(0.49,6.,1.4));
#13566=CARTESIAN_POINT('',(0.49,5.87783208277129,1.));
#13567=CARTESIAN_POINT('Origin',(0.,6.,1.));
#13568=CARTESIAN_POINT('',(-0.505,6.,1.8));
#13569=CARTESIAN_POINT('Origin',(0.,6.,1.8));
#13570=CARTESIAN_POINT('',(-0.505,6.,1.));
#13571=CARTESIAN_POINT('',(-0.505,6.,1.));
#13572=CARTESIAN_POINT('Origin',(0.,6.,1.));
#13573=CARTESIAN_POINT('Origin',(0.,6.,1.));
#13574=CARTESIAN_POINT('',(-0.9,6.,1.8));
#13575=CARTESIAN_POINT('Origin',(0.,6.,1.8));
#13576=CARTESIAN_POINT('',(-0.9,6.,1.));
#13577=CARTESIAN_POINT('',(-0.9,6.,1.));
#13578=CARTESIAN_POINT('Origin',(0.,6.,1.));
#13579=CARTESIAN_POINT('Origin',(0.,6.,1.8));
#13580=CARTESIAN_POINT('Origin',(0.,6.,1.));
#13581=CARTESIAN_POINT('',(0.,0.,0.));
#13582=CARTESIAN_POINT('Origin',(0.,9.,7.1));
#13583=CARTESIAN_POINT('',(-0.165,9.,7.1));
#13584=CARTESIAN_POINT('Origin',(0.,9.,7.1));
#13585=CARTESIAN_POINT('',(-0.165,9.,8.));
#13586=CARTESIAN_POINT('',(-0.165,9.,7.1));
#13587=CARTESIAN_POINT('Origin',(0.,9.,8.));
#13588=CARTESIAN_POINT('Origin',(0.,9.,7.1));
#13589=CARTESIAN_POINT('Origin',(0.,9.,6.));
#13590=CARTESIAN_POINT('',(-0.7,9.,6.));
#13591=CARTESIAN_POINT('Origin',(0.,9.,6.));
#13592=CARTESIAN_POINT('',(-0.3,9.,6.));
#13593=CARTESIAN_POINT('Origin',(0.,9.,6.));
#13594=CARTESIAN_POINT('Origin',(0.,9.,5.6));
#13595=CARTESIAN_POINT('',(-0.7,9.,5.6));
#13596=CARTESIAN_POINT('Origin',(0.,9.,5.6));
#13597=CARTESIAN_POINT('',(-0.3,9.,5.6));
#13598=CARTESIAN_POINT('Origin',(0.,9.,5.6));
#13599=CARTESIAN_POINT('Origin',(0.,9.,5.6));
#13600=CARTESIAN_POINT('',(-0.7,9.,5.6));
#13601=CARTESIAN_POINT('Origin',(0.,9.,4.8));
#13602=CARTESIAN_POINT('',(-0.3,9.,4.8));
#13603=CARTESIAN_POINT('',(-0.3,9.,4.8));
#13604=CARTESIAN_POINT('Origin',(0.,9.,4.8));
#13605=CARTESIAN_POINT('Origin',(0.,9.,4.8));
#13606=CARTESIAN_POINT('',(-0.3,9.,8.));
#13607=CARTESIAN_POINT('Origin',(0.,9.,8.));
#13608=CARTESIAN_POINT('',(-0.3,9.,4.8));
#13609=CARTESIAN_POINT('Origin',(0.,9.,8.));
#13610=CARTESIAN_POINT('Origin',(0.,9.,4.8));
#13611=CARTESIAN_POINT('',(0.,0.,0.));
#13612=CARTESIAN_POINT('Origin',(0.,9.,6.));
#13613=CARTESIAN_POINT('',(-0.305,9.,6.2));
#13614=CARTESIAN_POINT('Origin',(0.,9.,6.2));
#13615=CARTESIAN_POINT('',(-0.305,9.,6.));
#13616=CARTESIAN_POINT('',(-0.305,9.,6.));
#13617=CARTESIAN_POINT('Origin',(0.,9.,6.));
#13618=CARTESIAN_POINT('Origin',(0.,9.,6.));
#13619=CARTESIAN_POINT('',(-0.5,9.,6.2));
#13620=CARTESIAN_POINT('Origin',(0.,9.,6.2));
#13621=CARTESIAN_POINT('',(-0.5,9.,6.));
#13622=CARTESIAN_POINT('',(-0.5,9.,6.));
#13623=CARTESIAN_POINT('Origin',(0.,9.,6.));
#13624=CARTESIAN_POINT('Origin',(0.,9.,6.2));
#13625=CARTESIAN_POINT('Origin',(0.,9.,6.));
#13626=CARTESIAN_POINT('',(0.,0.,0.));
#13627=CARTESIAN_POINT('Origin',(0.,9.,7.4));
#13628=CARTESIAN_POINT('',(-0.305,9.,8.));
#13629=CARTESIAN_POINT('Origin',(0.,9.,8.));
#13630=CARTESIAN_POINT('',(-0.305,9.,7.4));
#13631=CARTESIAN_POINT('',(-0.305,9.,7.4));
#13632=CARTESIAN_POINT('Origin',(0.,9.,7.4));
#13633=CARTESIAN_POINT('Origin',(0.,9.,7.4));
#13634=CARTESIAN_POINT('',(-0.5,9.,8.));
#13635=CARTESIAN_POINT('Origin',(0.,9.,8.));
#13636=CARTESIAN_POINT('',(-0.5,9.,7.4));
#13637=CARTESIAN_POINT('',(-0.5,9.,7.4));
#13638=CARTESIAN_POINT('Origin',(0.,9.,7.4));
#13639=CARTESIAN_POINT('Origin',(0.,9.,8.));
#13640=CARTESIAN_POINT('Origin',(0.,9.,7.4));
#13641=CARTESIAN_POINT('',(0.,0.,0.));
#13642=CARTESIAN_POINT('Origin',(0.,9.,8.));
#13643=CARTESIAN_POINT('',(-0.225,9.,8.2));
#13644=CARTESIAN_POINT('Origin',(0.,9.,8.2));
#13645=CARTESIAN_POINT('',(-0.225,9.,8.));
#13646=CARTESIAN_POINT('',(-0.225,9.,8.));
#13647=CARTESIAN_POINT('Origin',(0.,9.,8.));
#13648=CARTESIAN_POINT('Origin',(0.,9.,8.));
#13649=CARTESIAN_POINT('',(-0.5,9.,8.2));
#13650=CARTESIAN_POINT('Origin',(0.,9.,8.2));
#13651=CARTESIAN_POINT('',(-0.5,9.,8.));
#13652=CARTESIAN_POINT('',(-0.5,9.,8.));
#13653=CARTESIAN_POINT('Origin',(0.,9.,8.));
#13654=CARTESIAN_POINT('Origin',(0.,9.,8.2));
#13655=CARTESIAN_POINT('Origin',(0.,9.,8.));
#13656=CARTESIAN_POINT('',(0.,0.,0.));
#13657=CARTESIAN_POINT('Origin',(0.3,0.4,0.));
#13658=CARTESIAN_POINT('',(-0.3,0.4,-3.67394039744206E-17));
#13659=CARTESIAN_POINT('Origin',(0.,0.4,0.));
#13660=CARTESIAN_POINT('Origin',(0.,0.375,0.));
#13661=CARTESIAN_POINT('',(-0.35,0.35,-4.28626379701573E-17));
#13662=CARTESIAN_POINT('Origin',(0.,0.35,0.));
#13663=CARTESIAN_POINT('',(-0.325,0.375,-3.9801020972289E-17));
#13664=CARTESIAN_POINT('Origin',(0.,0.19,0.));
#13665=CARTESIAN_POINT('',(-0.35,0.03,-4.28626379701574E-17));
#13666=CARTESIAN_POINT('Origin',(0.,0.03,0.));
#13667=CARTESIAN_POINT('',(-0.35,0.19,-4.28626379701574E-17));
#13668=CARTESIAN_POINT('Origin',(0.,0.0149999999999999,0.));
#13669=CARTESIAN_POINT('',(-0.32,-3.29597460435593E-17,-3.91886975727153E-17));
#13670=CARTESIAN_POINT('Origin',(0.,0.,0.));
#13671=CARTESIAN_POINT('',(-0.335,0.0149999999999999,-4.10256677714363E-17));
#13672=CARTESIAN_POINT('Origin',(0.22,0.,0.));
#13673=CARTESIAN_POINT('',(-0.22,-6.93889390390723E-18,-2.69422295812418E-17));
#13674=CARTESIAN_POINT('Origin',(0.,0.,0.));
#13675=CARTESIAN_POINT('Origin',(0.,-0.02,0.));
#13676=CARTESIAN_POINT('',(-0.1954,-0.0492,2.39295984553393E-17));
#13677=CARTESIAN_POINT('Origin',(0.,-0.0492,0.));
#13678=CARTESIAN_POINT('',(-0.21,-0.02,-2.57175827820944E-17));
#13679=CARTESIAN_POINT('Origin',(0.,-0.8,0.));
#13680=CARTESIAN_POINT('',(-0.1954,-1.5646,2.39295984553393E-17));
#13681=CARTESIAN_POINT('Origin',(0.,-1.5646,0.));
#13682=CARTESIAN_POINT('',(-0.1954,-0.8,-2.39295984553393E-17));
#13683=CARTESIAN_POINT('Origin',(0.,-1.58,0.));
#13684=CARTESIAN_POINT('',(-0.16,-1.6,-1.95943487863577E-17));
#13685=CARTESIAN_POINT('Origin',(0.,-1.6,0.));
#13686=CARTESIAN_POINT('',(-0.18,-1.58,-2.20436423846524E-17));
#13687=CARTESIAN_POINT('Origin',(0.,-1.6,0.));
#13688=CARTESIAN_POINT('Origin',(0.0866025403784439,-0.4,-0.15));
#13689=CARTESIAN_POINT('',(0.173205080756888,-0.4,0.));
#13690=CARTESIAN_POINT('',(0.0866025403784439,-0.4,-0.15));
#13691=CARTESIAN_POINT('',(0.173205080756888,-0.4,0.));
#13692=CARTESIAN_POINT('',(0.0866025403784439,-0.64,-0.15));
#13693=CARTESIAN_POINT('',(0.0866025403784439,-0.4,-0.15));
#13694=CARTESIAN_POINT('',(0.173205080756888,-0.64,0.));
#13695=CARTESIAN_POINT('',(0.173205080756888,-0.64,0.));
#13696=CARTESIAN_POINT('',(0.173205080756888,-0.4,0.));
#13697=CARTESIAN_POINT('Origin',(-0.0866025403784438,-0.4,-0.15));
#13698=CARTESIAN_POINT('',(-0.0866025403784438,-0.4,-0.15));
#13699=CARTESIAN_POINT('',(0.0866025403784439,-0.4,-0.15));
#13700=CARTESIAN_POINT('',(-0.0866025403784438,-0.64,-0.15));
#13701=CARTESIAN_POINT('',(-0.0866025403784438,-0.4,-0.15));
#13702=CARTESIAN_POINT('',(0.0866025403784439,-0.64,-0.15));
#13703=CARTESIAN_POINT('Origin',(-0.173205080756888,-0.4,-2.77555756156289E-17));
#13704=CARTESIAN_POINT('',(-0.173205080756888,-0.4,-2.12115047744981E-17));
#13705=CARTESIAN_POINT('',(-0.0866025403784438,-0.4,-0.15));
#13706=CARTESIAN_POINT('',(-0.173205080756888,-0.64,-2.77555756156289E-17));
#13707=CARTESIAN_POINT('',(-0.173205080756888,-0.4,-2.12115047744981E-17));
#13708=CARTESIAN_POINT('',(-0.0866025403784438,-0.64,-0.15));
#13709=CARTESIAN_POINT('Origin',(-0.0866025403784439,-0.4,0.15));
#13710=CARTESIAN_POINT('',(-0.0866025403784439,-0.4,0.15));
#13711=CARTESIAN_POINT('',(-0.173205080756888,-0.4,-2.12115047744981E-17));
#13712=CARTESIAN_POINT('',(-0.0866025403784439,-0.64,0.15));
#13713=CARTESIAN_POINT('',(-0.0866025403784439,-0.4,0.15));
#13714=CARTESIAN_POINT('',(-0.173205080756888,-0.64,-2.12115047744981E-17));
#13715=CARTESIAN_POINT('Origin',(0.0866025403784439,-0.4,0.15));
#13716=CARTESIAN_POINT('',(0.0866025403784439,-0.4,0.15));
#13717=CARTESIAN_POINT('',(-0.0866025403784439,-0.4,0.15));
#13718=CARTESIAN_POINT('',(0.0866025403784439,-0.64,0.15));
#13719=CARTESIAN_POINT('',(0.0866025403784439,-0.4,0.15));
#13720=CARTESIAN_POINT('',(-0.0866025403784439,-0.64,0.15));
#13721=CARTESIAN_POINT('Origin',(0.173205080756888,-0.4,0.));
#13722=CARTESIAN_POINT('',(0.0866025403784439,-0.4,0.15));
#13723=CARTESIAN_POINT('',(0.0866025403784439,-0.64,0.15));
#13724=CARTESIAN_POINT('Origin',(0.,-0.4,-2.77555756156289E-17));
#13725=CARTESIAN_POINT('Origin',(0.,-0.64,-2.77555756156289E-17));
#13726=CARTESIAN_POINT('',(0.,0.,0.));
#13727=CARTESIAN_POINT('',(0.,0.,0.));
#13728=CARTESIAN_POINT('Origin',(0.,12.,6.3));
#13729=CARTESIAN_POINT('',(-0.25,12.,6.4));
#13730=CARTESIAN_POINT('Origin',(0.,12.,6.4));
#13731=CARTESIAN_POINT('',(-0.25,12.,7.2));
#13732=CARTESIAN_POINT('',(-0.25,12.,6.3));
#13733=CARTESIAN_POINT('Origin',(0.,12.,7.2));
#13734=CARTESIAN_POINT('Origin',(-0.71,2.2,6.3));
#13735=CARTESIAN_POINT('',(-0.71,2.2,6.4));
#13736=CARTESIAN_POINT('',(0.71,2.2,6.4));
#13737=CARTESIAN_POINT('',(-0.355,2.2,6.4));
#13738=CARTESIAN_POINT('',(-0.71,2.2,7.2));
#13739=CARTESIAN_POINT('',(-0.71,2.2,6.3));
#13740=CARTESIAN_POINT('',(0.71,2.2,7.2));
#13741=CARTESIAN_POINT('',(-0.355,2.2,7.2));
#13742=CARTESIAN_POINT('',(0.71,2.2,6.3));
#13743=CARTESIAN_POINT('Origin',(0.71,2.2,6.3));
#13744=CARTESIAN_POINT('',(0.71,9.8,6.4));
#13745=CARTESIAN_POINT('',(0.71,1.1,6.4));
#13746=CARTESIAN_POINT('',(0.71,9.8,7.2));
#13747=CARTESIAN_POINT('',(0.71,1.1,7.2));
#13748=CARTESIAN_POINT('',(0.71,9.8,6.3));
#13749=CARTESIAN_POINT('Origin',(0.71,9.8,6.3));
#13750=CARTESIAN_POINT('',(-0.71,9.8,6.4));
#13751=CARTESIAN_POINT('',(0.355,9.8,6.4));
#13752=CARTESIAN_POINT('',(-0.71,9.8,7.2));
#13753=CARTESIAN_POINT('',(0.355,9.8,7.2));
#13754=CARTESIAN_POINT('',(-0.71,9.8,6.3));
#13755=CARTESIAN_POINT('Origin',(-0.71,9.8,6.3));
#13756=CARTESIAN_POINT('',(-0.71,4.9,6.4));
#13757=CARTESIAN_POINT('',(-0.71,4.9,7.2));
#13758=CARTESIAN_POINT('Origin',(0.,12.,6.4));
#13759=CARTESIAN_POINT('',(-1.2,12.,6.4));
#13760=CARTESIAN_POINT('',(-1.2,12.,7.2));
#13761=CARTESIAN_POINT('',(-1.2,12.,6.4));
#13762=CARTESIAN_POINT('',(1.2,12.,7.2));
#13763=CARTESIAN_POINT('Origin',(0.,12.,7.2));
#13764=CARTESIAN_POINT('',(1.2,12.,6.4));
#13765=CARTESIAN_POINT('',(1.2,12.,6.4));
#13766=CARTESIAN_POINT('Origin',(0.,12.,6.4));
#13767=CARTESIAN_POINT('Origin',(0.,0.,6.4));
#13768=CARTESIAN_POINT('',(1.2,0.,6.4));
#13769=CARTESIAN_POINT('',(1.2,12.,6.4));
#13770=CARTESIAN_POINT('',(-1.2,-1.46957615897682E-16,6.4));
#13771=CARTESIAN_POINT('Origin',(0.,0.,6.4));
#13772=CARTESIAN_POINT('',(-1.2,0.,6.4));
#13773=CARTESIAN_POINT('',(-0.7,-8.57252759403147E-17,6.4));
#13774=CARTESIAN_POINT('Origin',(0.,0.,6.4));
#13775=CARTESIAN_POINT('Origin',(-1.2,12.,6.4));
#13776=CARTESIAN_POINT('',(-1.2,-1.46957615897682E-16,7.2));
#13777=CARTESIAN_POINT('',(-1.2,0.,6.4));
#13778=CARTESIAN_POINT('',(-1.2,0.,7.2));
#13779=CARTESIAN_POINT('Origin',(1.2,0.,6.4));
#13780=CARTESIAN_POINT('',(1.2,0.,7.2));
#13781=CARTESIAN_POINT('',(1.2,12.,7.2));
#13782=CARTESIAN_POINT('',(1.2,0.,6.4));
#13783=CARTESIAN_POINT('Origin',(0.,0.,6.4));
#13784=CARTESIAN_POINT('Origin',(0.,0.,7.2));
#13785=CARTESIAN_POINT('Origin',(0.,0.,2.95));
#13786=CARTESIAN_POINT('',(-0.7,-8.57252759403147E-17,2.95));
#13787=CARTESIAN_POINT('Origin',(0.,0.,2.95));
#13788=CARTESIAN_POINT('',(-0.5,6.12323399573677E-17,2.95));
#13789=CARTESIAN_POINT('Origin',(0.,0.,2.95));
#13790=CARTESIAN_POINT('Origin',(0.,0.,2.95));
#13791=CARTESIAN_POINT('',(-0.7,-8.57252759403147E-17,2.95));
#13792=CARTESIAN_POINT('Origin',(0.,0.,1.));
#13793=CARTESIAN_POINT('',(-0.5,-6.12323399573677E-17,1.));
#13794=CARTESIAN_POINT('',(-0.5,-6.12323399573677E-17,1.));
#13795=CARTESIAN_POINT('Origin',(0.,0.,1.));
#13796=CARTESIAN_POINT('Origin',(0.,0.,7.2));
#13797=CARTESIAN_POINT('Origin',(0.,0.,1.));
#13798=CARTESIAN_POINT('',(0.,0.,0.));
#13799=CARTESIAN_POINT('Origin',(0.,0.,1.8));
#13800=CARTESIAN_POINT('',(-0.505,-6.18446633569413E-17,2.05));
#13801=CARTESIAN_POINT('Origin',(0.,0.,2.05));
#13802=CARTESIAN_POINT('',(-0.505,-6.18446633569413E-17,1.8));
#13803=CARTESIAN_POINT('',(-0.505,-6.18446633569413E-17,1.8));
#13804=CARTESIAN_POINT('Origin',(0.,0.,1.8));
#13805=CARTESIAN_POINT('Origin',(0.,0.,1.8));
#13806=CARTESIAN_POINT('',(-0.7,-8.57252759403147E-17,2.05));
#13807=CARTESIAN_POINT('Origin',(0.,0.,2.05));
#13808=CARTESIAN_POINT('',(-0.7,-8.57252759403147E-17,1.8));
#13809=CARTESIAN_POINT('',(-0.7,-8.57252759403147E-17,1.8));
#13810=CARTESIAN_POINT('Origin',(0.,0.,1.8));
#13811=CARTESIAN_POINT('Origin',(0.,0.,2.05));
#13812=CARTESIAN_POINT('Origin',(0.,0.,1.8));
#13813=CARTESIAN_POINT('',(0.,0.,0.));
#13814=CARTESIAN_POINT('Origin',(0.49,0.,1.4));
#13815=CARTESIAN_POINT('',(0.49,0.122167917228706,1.28909463493591));
#13816=CARTESIAN_POINT('',(0.49,0.122167917228706,1.51090536506409));
#13817=CARTESIAN_POINT('',(0.49,0.122167917228706,1.));
#13818=CARTESIAN_POINT('Origin',(0.49,0.,1.4));
#13819=CARTESIAN_POINT('Origin',(0.49,0.,1.4));
#13820=CARTESIAN_POINT('',(0.49,-0.122167917228706,1.28909463493591));
#13821=CARTESIAN_POINT('Ctrl Pts',(0.49,-0.122167917228706,1.28909463493591));
#13822=CARTESIAN_POINT('Ctrl Pts',(0.490448531679987,-0.120368913626296,
1.28711294069536));
#13823=CARTESIAN_POINT('Ctrl Pts',(0.490895245371685,-0.118534896565231,
1.28518965877367));
#13824=CARTESIAN_POINT('Ctrl Pts',(0.494795015531646,-0.102111993019358,
1.2687667552278));
#13825=CARTESIAN_POINT('Ctrl Pts',(0.498442514607594,-0.0836597150224318,
1.25609154388858));
#13826=CARTESIAN_POINT('Ctrl Pts',(0.50357781976106,-0.0430495960471595,
1.23920409039234));
#13827=CARTESIAN_POINT('Ctrl Pts',(0.505,-0.020880094330741,1.235));
#13828=CARTESIAN_POINT('Ctrl Pts',(0.505,0.020880094330741,1.235));
#13829=CARTESIAN_POINT('Ctrl Pts',(0.50357781976106,0.0430495960471595,
1.23920409039234));
#13830=CARTESIAN_POINT('Ctrl Pts',(0.498442514607594,0.0836597150224318,
1.25609154388858));
#13831=CARTESIAN_POINT('Ctrl Pts',(0.494795015531646,0.102111993019358,
1.2687667552278));
#13832=CARTESIAN_POINT('Ctrl Pts',(0.490895245371684,0.118534896565231,
1.28518965877367));
#13833=CARTESIAN_POINT('Ctrl Pts',(0.490448531679987,0.120368913626296,
1.28711294069536));
#13834=CARTESIAN_POINT('Ctrl Pts',(0.49,0.122167917228706,1.28909463493591));
#13835=CARTESIAN_POINT('',(0.49,-0.122167917228706,1.51090536506409));
#13836=CARTESIAN_POINT('Origin',(0.49,0.,1.4));
#13837=CARTESIAN_POINT('',(0.505,-1.70422299968729E-17,1.565));
#13838=CARTESIAN_POINT('Ctrl Pts',(0.505,-6.93889390390723E-18,1.565));
#13839=CARTESIAN_POINT('Ctrl Pts',(0.505,-0.020880094330741,1.565));
#13840=CARTESIAN_POINT('Ctrl Pts',(0.50357781976106,-0.0430495960471595,
1.56079590960766));
#13841=CARTESIAN_POINT('Ctrl Pts',(0.498442514607594,-0.0836597150224318,
1.54390845611142));
#13842=CARTESIAN_POINT('Ctrl Pts',(0.494795015531646,-0.102111993019358,
1.5312332447722));
#13843=CARTESIAN_POINT('Ctrl Pts',(0.490895245371684,-0.118534896565231,
1.51481034122633));
#13844=CARTESIAN_POINT('Ctrl Pts',(0.490448531679987,-0.120368913626296,
1.51288705930464));
#13845=CARTESIAN_POINT('Ctrl Pts',(0.49,-0.122167917228706,1.51090536506409));
#13846=CARTESIAN_POINT('',(0.9,-2.02066721859313E-17,1.565));
#13847=CARTESIAN_POINT('',(0.49,-2.02066721859313E-17,1.565));
#13848=CARTESIAN_POINT('',(0.884745726183518,0.165,1.4));
#13849=CARTESIAN_POINT('Ctrl Pts',(0.884745726183518,0.165,1.4));
#13850=CARTESIAN_POINT('Ctrl Pts',(0.884745726183518,0.165,1.37923124059256));
#13851=CARTESIAN_POINT('Ctrl Pts',(0.885552759505264,0.160839719007584,
1.35711110492666));
#13852=CARTESIAN_POINT('Ctrl Pts',(0.888448648150043,0.143986470216691,
1.31647293736623));
#13853=CARTESIAN_POINT('Ctrl Pts',(0.890493604851638,0.131295993814186,
1.29795075602263));
#13854=CARTESIAN_POINT('Ctrl Pts',(0.89431723432394,0.102049819008125,1.26870458121656));
#13855=CARTESIAN_POINT('Ctrl Pts',(0.896347088899543,0.0835273920906824,
1.25601365401642));
#13856=CARTESIAN_POINT('Ctrl Pts',(0.899208271860583,0.0428883760934127,
1.23916007816136));
#13857=CARTESIAN_POINT('Ctrl Pts',(0.9,0.0207679427235068,1.235));
#13858=CARTESIAN_POINT('Ctrl Pts',(0.9,-0.0207679427235068,1.235));
#13859=CARTESIAN_POINT('Ctrl Pts',(0.899208271860583,-0.0428883760934127,
1.23916007816136));
#13860=CARTESIAN_POINT('Ctrl Pts',(0.896347088899543,-0.0835273920906823,
1.25601365401642));
#13861=CARTESIAN_POINT('Ctrl Pts',(0.89431723432394,-0.102049819008125,
1.26870458121656));
#13862=CARTESIAN_POINT('Ctrl Pts',(0.890493604851638,-0.131295993814186,
1.29795075602263));
#13863=CARTESIAN_POINT('Ctrl Pts',(0.888448648150043,-0.143986470216691,
1.31647293736623));
#13864=CARTESIAN_POINT('Ctrl Pts',(0.885552759505264,-0.160839719007584,
1.35711110492666));
#13865=CARTESIAN_POINT('Ctrl Pts',(0.884745726183518,-0.165,1.37923124059256));
#13866=CARTESIAN_POINT('Ctrl Pts',(0.884745726183518,-0.165,1.42076875940744));
#13867=CARTESIAN_POINT('Ctrl Pts',(0.885552759505264,-0.160839719007584,
1.44288889507334));
#13868=CARTESIAN_POINT('Ctrl Pts',(0.888448648150043,-0.14398647021669,
1.48352706263377));
#13869=CARTESIAN_POINT('Ctrl Pts',(0.890493604851638,-0.131295993814186,
1.50204924397737));
#13870=CARTESIAN_POINT('Ctrl Pts',(0.89431723432394,-0.102049819008125,
1.53129541878344));
#13871=CARTESIAN_POINT('Ctrl Pts',(0.896347088899543,-0.0835273920906824,
1.54398634598358));
#13872=CARTESIAN_POINT('Ctrl Pts',(0.899208271860583,-0.0428883760934128,
1.56083992183864));
#13873=CARTESIAN_POINT('Ctrl Pts',(0.9,-0.0207679427235068,1.565));
#13874=CARTESIAN_POINT('Ctrl Pts',(0.9,-6.93889390390723E-18,1.565));
#13875=CARTESIAN_POINT('Ctrl Pts',(0.9,-3.46944695195361E-17,1.565));
#13876=CARTESIAN_POINT('Ctrl Pts',(0.9,0.0207679427235068,1.565));
#13877=CARTESIAN_POINT('Ctrl Pts',(0.899208271860583,0.0428883760934127,
1.56083992183864));
#13878=CARTESIAN_POINT('Ctrl Pts',(0.896347088899543,0.0835273920906824,
1.54398634598358));
#13879=CARTESIAN_POINT('Ctrl Pts',(0.89431723432394,0.102049819008125,1.53129541878344));
#13880=CARTESIAN_POINT('Ctrl Pts',(0.890493604851638,0.131295993814186,
1.50204924397737));
#13881=CARTESIAN_POINT('Ctrl Pts',(0.888448648150043,0.143986470216691,
1.48352706263377));
#13882=CARTESIAN_POINT('Ctrl Pts',(0.885552759505264,0.160839719007584,
1.44288889507334));
#13883=CARTESIAN_POINT('Ctrl Pts',(0.884745726183518,0.165,1.42076875940744));
#13884=CARTESIAN_POINT('Ctrl Pts',(0.884745726183518,0.165,1.4));
#13885=CARTESIAN_POINT('Ctrl Pts',(0.49,0.122167917228706,1.51090536506409));
#13886=CARTESIAN_POINT('Ctrl Pts',(0.490448531679987,0.120368913626296,
1.51288705930464));
#13887=CARTESIAN_POINT('Ctrl Pts',(0.490895245371685,0.118534896565231,
1.51481034122633));
#13888=CARTESIAN_POINT('Ctrl Pts',(0.494795015531646,0.102111993019358,
1.5312332447722));
#13889=CARTESIAN_POINT('Ctrl Pts',(0.498442514607594,0.0836597150224318,
1.54390845611142));
#13890=CARTESIAN_POINT('Ctrl Pts',(0.50357781976106,0.0430495960471594,
1.56079590960766));
#13891=CARTESIAN_POINT('Ctrl Pts',(0.505,0.020880094330741,1.565));
#13892=CARTESIAN_POINT('Ctrl Pts',(0.505,0.,1.565));
#13893=CARTESIAN_POINT('Origin',(0.49,0.,1.4));
#13894=CARTESIAN_POINT('',(0.49,-0.122167917228706,1.));
#13895=CARTESIAN_POINT('Origin',(0.,0.,1.));
#13896=CARTESIAN_POINT('',(-0.505,-6.18446633569413E-17,1.8));
#13897=CARTESIAN_POINT('Origin',(0.,0.,1.8));
#13898=CARTESIAN_POINT('',(-0.505,-6.18446633569413E-17,1.));
#13899=CARTESIAN_POINT('',(-0.505,-6.18446633569413E-17,1.));
#13900=CARTESIAN_POINT('Origin',(0.,0.,1.));
#13901=CARTESIAN_POINT('Origin',(0.,0.,1.));
#13902=CARTESIAN_POINT('',(-0.9,-1.10218211923262E-16,1.8));
#13903=CARTESIAN_POINT('Origin',(0.,0.,1.8));
#13904=CARTESIAN_POINT('',(-0.9,-1.10218211923262E-16,1.));
#13905=CARTESIAN_POINT('',(-0.9,-1.10218211923262E-16,1.));
#13906=CARTESIAN_POINT('Origin',(0.,0.,1.));
#13907=CARTESIAN_POINT('Origin',(0.,0.,1.8));
#13908=CARTESIAN_POINT('Origin',(0.,0.,1.));
#13909=CARTESIAN_POINT('',(0.,0.,0.));
#13910=CARTESIAN_POINT('Origin',(0.,12.,8.9));
#13911=CARTESIAN_POINT('',(-0.165,12.,8.9));
#13912=CARTESIAN_POINT('Origin',(0.,12.,8.9));
#13913=CARTESIAN_POINT('',(-0.165,12.,9.8));
#13914=CARTESIAN_POINT('',(-0.165,12.,8.9));
#13915=CARTESIAN_POINT('Origin',(0.,12.,9.8));
#13916=CARTESIAN_POINT('Origin',(0.,12.,8.9));
#13917=CARTESIAN_POINT('Origin',(0.,12.,7.6));
#13918=CARTESIAN_POINT('',(-0.7,12.,7.6));
#13919=CARTESIAN_POINT('Origin',(0.,12.,7.6));
#13920=CARTESIAN_POINT('',(-0.3,12.,7.6));
#13921=CARTESIAN_POINT('Origin',(0.,12.,7.6));
#13922=CARTESIAN_POINT('Origin',(0.,12.,7.2));
#13923=CARTESIAN_POINT('',(-0.7,12.,7.2));
#13924=CARTESIAN_POINT('Origin',(0.,12.,7.2));
#13925=CARTESIAN_POINT('',(-0.3,12.,7.2));
#13926=CARTESIAN_POINT('Origin',(0.,12.,7.2));
#13927=CARTESIAN_POINT('Origin',(0.,12.,7.2));
#13928=CARTESIAN_POINT('',(-0.7,12.,7.2));
#13929=CARTESIAN_POINT('Origin',(0.,12.,6.4));
#13930=CARTESIAN_POINT('',(-0.3,12.,6.4));
#13931=CARTESIAN_POINT('',(-0.3,12.,6.4));
#13932=CARTESIAN_POINT('Origin',(0.,12.,6.4));
#13933=CARTESIAN_POINT('Origin',(0.,12.,6.4));
#13934=CARTESIAN_POINT('',(-0.3,12.,9.8));
#13935=CARTESIAN_POINT('Origin',(0.,12.,9.8));
#13936=CARTESIAN_POINT('',(-0.3,12.,6.4));
#13937=CARTESIAN_POINT('Origin',(0.,12.,9.8));
#13938=CARTESIAN_POINT('Origin',(0.,12.,6.4));
#13939=CARTESIAN_POINT('',(0.,0.,0.));
#13940=CARTESIAN_POINT('Origin',(0.,12.,7.6));
#13941=CARTESIAN_POINT('',(-0.305,12.,8.4));
#13942=CARTESIAN_POINT('Origin',(0.,12.,8.4));
#13943=CARTESIAN_POINT('',(-0.305,12.,7.6));
#13944=CARTESIAN_POINT('',(-0.305,12.,7.6));
#13945=CARTESIAN_POINT('Origin',(0.,12.,7.6));
#13946=CARTESIAN_POINT('Origin',(0.,12.,7.6));
#13947=CARTESIAN_POINT('',(-0.5,12.,8.4));
#13948=CARTESIAN_POINT('Origin',(0.,12.,8.4));
#13949=CARTESIAN_POINT('',(-0.5,12.,7.6));
#13950=CARTESIAN_POINT('',(-0.5,12.,7.6));
#13951=CARTESIAN_POINT('Origin',(0.,12.,7.6));
#13952=CARTESIAN_POINT('Origin',(0.,12.,8.4));
#13953=CARTESIAN_POINT('Origin',(0.,12.,7.6));
#13954=CARTESIAN_POINT('',(0.,0.,0.));
#13955=CARTESIAN_POINT('Origin',(0.,12.,9.2));
#13956=CARTESIAN_POINT('',(-0.305,12.,9.8));
#13957=CARTESIAN_POINT('Origin',(0.,12.,9.8));
#13958=CARTESIAN_POINT('',(-0.305,12.,9.2));
#13959=CARTESIAN_POINT('',(-0.305,12.,9.2));
#13960=CARTESIAN_POINT('Origin',(0.,12.,9.2));
#13961=CARTESIAN_POINT('Origin',(0.,12.,9.2));
#13962=CARTESIAN_POINT('',(-0.5,12.,9.8));
#13963=CARTESIAN_POINT('Origin',(0.,12.,9.8));
#13964=CARTESIAN_POINT('',(-0.5,12.,9.2));
#13965=CARTESIAN_POINT('',(-0.5,12.,9.2));
#13966=CARTESIAN_POINT('Origin',(0.,12.,9.2));
#13967=CARTESIAN_POINT('Origin',(0.,12.,9.8));
#13968=CARTESIAN_POINT('Origin',(0.,12.,9.2));
#13969=CARTESIAN_POINT('',(0.,0.,0.));
#13970=CARTESIAN_POINT('Origin',(0.,12.,9.8));
#13971=CARTESIAN_POINT('',(-0.225,12.,10.));
#13972=CARTESIAN_POINT('Origin',(0.,12.,10.));
#13973=CARTESIAN_POINT('',(-0.225,12.,9.8));
#13974=CARTESIAN_POINT('',(-0.225,12.,9.8));
#13975=CARTESIAN_POINT('Origin',(0.,12.,9.8));
#13976=CARTESIAN_POINT('Origin',(0.,12.,9.8));
#13977=CARTESIAN_POINT('',(-0.5,12.,10.));
#13978=CARTESIAN_POINT('Origin',(0.,12.,10.));
#13979=CARTESIAN_POINT('',(-0.5,12.,9.8));
#13980=CARTESIAN_POINT('',(-0.5,12.,9.8));
#13981=CARTESIAN_POINT('Origin',(0.,12.,9.8));
#13982=CARTESIAN_POINT('Origin',(0.,12.,10.));
#13983=CARTESIAN_POINT('Origin',(0.,12.,9.8));
#13984=CARTESIAN_POINT('',(0.,0.,0.));
#13985=CARTESIAN_POINT('Origin',(0.,-0.4,0.));
#13986=CARTESIAN_POINT('',(-0.1954,-0.4,2.39295984553393E-17));
#13987=CARTESIAN_POINT('Origin',(0.,-0.4,0.));
#13988=CARTESIAN_POINT('Origin',(0.0577350269189626,0.,-0.1));
#13989=CARTESIAN_POINT('',(0.0577350269189626,0.,-0.1));
#13990=CARTESIAN_POINT('',(0.115470053837925,0.,0.));
#13991=CARTESIAN_POINT('',(0.0934187836487032,0.,-0.0381939203391614));
#13992=CARTESIAN_POINT('',(0.0577350269189626,-0.2,-0.1));
#13993=CARTESIAN_POINT('',(0.0577350269189626,0.,-0.1));
#13994=CARTESIAN_POINT('',(0.115470053837925,-0.2,0.));
#13995=CARTESIAN_POINT('',(0.115470053837925,-0.2,0.));
#13996=CARTESIAN_POINT('',(0.115470053837925,0.,0.));
#13997=CARTESIAN_POINT('Origin',(-0.0577350269189626,0.,-0.1));
#13998=CARTESIAN_POINT('',(-0.0577350269189626,0.,-0.1));
#13999=CARTESIAN_POINT('',(0.0561324865405187,0.,-0.1));
#14000=CARTESIAN_POINT('',(-0.0577350269189626,-0.2,-0.1));
#14001=CARTESIAN_POINT('',(-0.0577350269189626,0.,-0.1));
#14002=CARTESIAN_POINT('',(0.0577350269189626,-0.2,-0.1));
#14003=CARTESIAN_POINT('Origin',(-0.115470053837925,0.,-1.38777878078145E-17));
#14004=CARTESIAN_POINT('',(-0.115470053837925,0.,-1.41410031829988E-17));
#14005=CARTESIAN_POINT('',(-0.0797862971081845,0.,-0.0618060796608387));
#14006=CARTESIAN_POINT('',(-0.115470053837925,-0.2,-1.38777878078145E-17));
#14007=CARTESIAN_POINT('',(-0.115470053837925,0.,-1.41410031829988E-17));
#14008=CARTESIAN_POINT('',(-0.0577350269189626,-0.2,-0.1));
#14009=CARTESIAN_POINT('Origin',(-0.0577350269189626,0.,0.1));
#14010=CARTESIAN_POINT('',(-0.0577350269189626,0.,0.1));
#14011=CARTESIAN_POINT('',(-0.0509187836487033,0.,0.111806079660839));
#14012=CARTESIAN_POINT('',(-0.0577350269189626,-0.2,0.1));
#14013=CARTESIAN_POINT('',(-0.0577350269189626,0.,0.1));
#14014=CARTESIAN_POINT('',(-0.115470053837925,-0.2,-1.41410031829988E-17));
#14015=CARTESIAN_POINT('Origin',(0.0577350269189626,0.,0.1));
#14016=CARTESIAN_POINT('',(0.0577350269189626,0.,0.1));
#14017=CARTESIAN_POINT('',(0.113867513459481,0.,0.1));
#14018=CARTESIAN_POINT('',(0.0577350269189626,-0.2,0.1));
#14019=CARTESIAN_POINT('',(0.0577350269189626,0.,0.1));
#14020=CARTESIAN_POINT('',(-0.0577350269189626,-0.2,0.1));
#14021=CARTESIAN_POINT('Origin',(0.115470053837925,0.,0.));
#14022=CARTESIAN_POINT('',(0.122286297108185,0.,-0.0118060796608386));
#14023=CARTESIAN_POINT('',(0.0577350269189626,-0.2,0.1));
#14024=CARTESIAN_POINT('Origin',(0.,-0.2,0.));
#14025=CARTESIAN_POINT('Origin',(0.17,0.,0.));
#14026=CARTESIAN_POINT('',(-0.17,-8.67361737988404E-18,-2.0818995585505E-17));
#14027=CARTESIAN_POINT('Origin',(0.,0.,0.));
#14028=CARTESIAN_POINT('Origin',(0.,-0.015,0.));
#14029=CARTESIAN_POINT('',(-0.1954,-0.0254,-2.39295984553393E-17));
#14030=CARTESIAN_POINT('Origin',(0.,-0.0254,0.));
#14031=CARTESIAN_POINT('',(-0.185,-0.015,-2.2655965784226E-17));
#14032=CARTESIAN_POINT('Origin',(0.,-0.2775,0.));
#14033=CARTESIAN_POINT('',(-0.1954,-0.2775,-2.39295984553393E-17));
#14034=CARTESIAN_POINT('',(0.,0.,0.));
#14035=CARTESIAN_POINT('',(0.,0.,0.));
#14036=CARTESIAN_POINT('Origin',(0.,9.,6.1));
#14037=CARTESIAN_POINT('',(-0.305,9.,6.2));
#14038=CARTESIAN_POINT('Origin',(0.,9.,6.2));
#14039=CARTESIAN_POINT('',(-0.305,9.,7.4));
#14040=CARTESIAN_POINT('',(-0.305,9.,6.1));
#14041=CARTESIAN_POINT('Origin',(0.,9.,7.4));
#14042=CARTESIAN_POINT('Origin',(0.,9.,7.2));
#14043=CARTESIAN_POINT('',(0.7,8.3,7.2));
#14044=CARTESIAN_POINT('',(0.7,9.7,7.2));
#14045=CARTESIAN_POINT('',(0.7,8.3,7.2));
#14046=CARTESIAN_POINT('',(1.1,9.7,7.2));
#14047=CARTESIAN_POINT('',(1.1,9.7,7.2));
#14048=CARTESIAN_POINT('',(1.1,8.3,7.2));
#14049=CARTESIAN_POINT('',(1.1,8.3,7.2));
#14050=CARTESIAN_POINT('',(-1.1,8.3,7.2));
#14051=CARTESIAN_POINT('Origin',(0.,9.,7.2));
#14052=CARTESIAN_POINT('',(-0.7,9.7,7.2));
#14053=CARTESIAN_POINT('',(-0.7,8.3,7.2));
#14054=CARTESIAN_POINT('',(-0.7,9.7,7.2));
#14055=CARTESIAN_POINT('',(-1.1,8.3,7.2));
#14056=CARTESIAN_POINT('',(-1.1,8.3,7.2));
#14057=CARTESIAN_POINT('',(-1.1,9.7,7.2));
#14058=CARTESIAN_POINT('',(-1.1,9.7,7.2));
#14059=CARTESIAN_POINT('',(1.1,9.7,7.2));
#14060=CARTESIAN_POINT('Origin',(1.1,8.3,7.2));
#14061=CARTESIAN_POINT('',(1.1,9.7,7.4));
#14062=CARTESIAN_POINT('',(1.1,9.7,7.2));
#14063=CARTESIAN_POINT('',(1.1,8.3,7.4));
#14064=CARTESIAN_POINT('',(1.1,8.3,7.4));
#14065=CARTESIAN_POINT('',(1.1,8.3,7.2));
#14066=CARTESIAN_POINT('Origin',(-1.1,9.7,7.2));
#14067=CARTESIAN_POINT('',(-1.1,8.3,7.4));
#14068=CARTESIAN_POINT('',(-1.1,8.3,7.2));
#14069=CARTESIAN_POINT('',(-1.1,9.7,7.4));
#14070=CARTESIAN_POINT('',(-1.1,9.7,7.4));
#14071=CARTESIAN_POINT('',(-1.1,9.7,7.2));
#14072=CARTESIAN_POINT('Origin',(0.,9.,7.4));
#14073=CARTESIAN_POINT('',(-1.1,8.3,7.4));
#14074=CARTESIAN_POINT('',(1.1,9.7,7.4));
#14075=CARTESIAN_POINT('Origin',(0.,9.,6.4));
#14076=CARTESIAN_POINT('',(-0.7,9.7,6.4));
#14077=CARTESIAN_POINT('',(-0.7,8.3,6.4));
#14078=CARTESIAN_POINT('',(-0.7,9.7,6.4));
#14079=CARTESIAN_POINT('',(-1.1,9.7,6.4));
#14080=CARTESIAN_POINT('',(1.1,9.7,6.4));
#14081=CARTESIAN_POINT('',(-1.1,8.3,6.4));
#14082=CARTESIAN_POINT('',(-1.1,9.7,6.4));
#14083=CARTESIAN_POINT('',(-1.1,8.3,6.4));
#14084=CARTESIAN_POINT('Origin',(0.,9.,6.4));
#14085=CARTESIAN_POINT('',(0.7,8.3,6.4));
#14086=CARTESIAN_POINT('',(0.7,9.7,6.4));
#14087=CARTESIAN_POINT('',(0.7,8.3,6.4));
#14088=CARTESIAN_POINT('',(1.1,8.3,6.4));
#14089=CARTESIAN_POINT('',(-1.1,8.3,6.4));
#14090=CARTESIAN_POINT('',(1.1,9.7,6.4));
#14091=CARTESIAN_POINT('',(1.1,8.3,6.4));
#14092=CARTESIAN_POINT('',(1.1,9.7,6.4));
#14093=CARTESIAN_POINT('Origin',(1.1,8.3,6.2));
#14094=CARTESIAN_POINT('',(1.1,8.3,6.2));
#14095=CARTESIAN_POINT('',(1.1,9.7,6.2));
#14096=CARTESIAN_POINT('',(1.1,8.3,6.2));
#14097=CARTESIAN_POINT('',(1.1,9.7,6.2));
#14098=CARTESIAN_POINT('',(1.1,8.3,6.2));
#14099=CARTESIAN_POINT('Origin',(-1.1,9.7,6.2));
#14100=CARTESIAN_POINT('',(-1.1,9.7,6.2));
#14101=CARTESIAN_POINT('',(-1.1,8.3,6.2));
#14102=CARTESIAN_POINT('',(-1.1,9.7,6.2));
#14103=CARTESIAN_POINT('',(-1.1,8.3,6.2));
#14104=CARTESIAN_POINT('',(-1.1,9.7,6.2));
#14105=CARTESIAN_POINT('Origin',(0.,9.,6.2));
#14106=CARTESIAN_POINT('',(1.1,9.7,6.2));
#14107=CARTESIAN_POINT('',(-1.1,8.3,6.2));
#14108=CARTESIAN_POINT('Origin',(0.7,9.7,6.4));
#14109=CARTESIAN_POINT('',(-0.7,9.7,6.4));
#14110=CARTESIAN_POINT('',(0.7,9.7,6.4));
#14111=CARTESIAN_POINT('Origin',(0.7,8.3,6.4));
#14112=CARTESIAN_POINT('',(0.7,8.3,6.4));
#14113=CARTESIAN_POINT('Origin',(-0.7,8.3,6.4));
#14114=CARTESIAN_POINT('',(-0.7,8.3,6.4));
#14115=CARTESIAN_POINT('Origin',(-0.7,9.7,6.4));
#14116=CARTESIAN_POINT('',(0.,0.,0.));
#14117=CARTESIAN_POINT('',(0.,0.,0.));
#14118=CARTESIAN_POINT('',(0.,0.,0.));
#14119=CARTESIAN_POINT('Origin',(0.,12.,8.3));
#14120=CARTESIAN_POINT('',(-0.5,12.,8.4));
#14121=CARTESIAN_POINT('Origin',(0.,12.,8.4));
#14122=CARTESIAN_POINT('',(-0.5,12.,9.2));
#14123=CARTESIAN_POINT('',(-0.5,12.,8.3));
#14124=CARTESIAN_POINT('Origin',(0.,12.,9.2));
#14125=CARTESIAN_POINT('Origin',(9.16515138991168,16.,8.3));
#14126=CARTESIAN_POINT('',(8.66515138991168,16.,8.4));
#14127=CARTESIAN_POINT('Origin',(9.16515138991168,16.,8.4));
#14128=CARTESIAN_POINT('',(8.66515138991168,16.,9.2));
#14129=CARTESIAN_POINT('',(8.66515138991168,16.,8.3));
#14130=CARTESIAN_POINT('Origin',(9.16515138991168,16.,9.2));
#14131=CARTESIAN_POINT('Origin',(9.16515138991168,16.,8.4));
#14132=CARTESIAN_POINT('',(8.39278786906151,16.2084576495596,9.2));
#14133=CARTESIAN_POINT('',(8.39278786906151,16.2084576495596,8.4));
#14134=CARTESIAN_POINT('',(8.39278786906151,16.2084576495596,8.4));
#14135=CARTESIAN_POINT('',(8.79278786906151,15.2919425105685,9.2));
#14136=CARTESIAN_POINT('Origin',(9.16515138991168,16.,9.2));
#14137=CARTESIAN_POINT('',(8.79278786906151,15.2919425105685,8.4));
#14138=CARTESIAN_POINT('',(8.79278786906151,15.2919425105685,8.4));
#14139=CARTESIAN_POINT('Origin',(9.16515138991168,16.,8.4));
#14140=CARTESIAN_POINT('Origin',(8.96515138991168,16.4582575694956,8.4));
#14141=CARTESIAN_POINT('',(0.372363520850169,12.7080574894315,8.4));
#14142=CARTESIAN_POINT('',(-0.2,12.4582575694956,8.4));
#14143=CARTESIAN_POINT('',(0.372363520850169,12.7080574894315,9.2));
#14144=CARTESIAN_POINT('',(0.372363520850169,12.7080574894315,8.4));
#14145=CARTESIAN_POINT('',(-0.2,12.4582575694956,9.2));
#14146=CARTESIAN_POINT('Origin',(0.,12.,8.4));
#14147=CARTESIAN_POINT('',(0.772363520850167,11.7915423504404,8.4));
#14148=CARTESIAN_POINT('',(9.36515138991168,15.5417424305044,8.4));
#14149=CARTESIAN_POINT('Origin',(0.,12.,8.4));
#14150=CARTESIAN_POINT('Origin',(0.199999999999999,11.5417424305044,8.4));
#14151=CARTESIAN_POINT('',(0.772363520850167,11.7915423504404,9.2));
#14152=CARTESIAN_POINT('',(9.36515138991168,15.5417424305044,9.2));
#14153=CARTESIAN_POINT('',(0.772363520850168,11.7915423504404,8.4));
#14154=CARTESIAN_POINT('Origin',(0.,12.,8.4));
#14155=CARTESIAN_POINT('Origin',(0.,12.,9.2));
#14156=CARTESIAN_POINT('Origin',(0.,12.,9.2));
#14157=CARTESIAN_POINT('',(0.,0.,0.));
#14158=CARTESIAN_POINT('Origin',(0.,12.,8.4));
#14159=CARTESIAN_POINT('',(-0.305,12.,9.2));
#14160=CARTESIAN_POINT('Origin',(0.,12.,9.2));
#14161=CARTESIAN_POINT('',(-0.305,12.,8.4));
#14162=CARTESIAN_POINT('',(-0.305,12.,8.4));
#14163=CARTESIAN_POINT('Origin',(0.,12.,8.4));
#14164=CARTESIAN_POINT('Origin',(0.,12.,8.4));
#14165=CARTESIAN_POINT('',(-0.5,12.,9.2));
#14166=CARTESIAN_POINT('Origin',(0.,12.,9.2));
#14167=CARTESIAN_POINT('',(-0.5,12.,8.4));
#14168=CARTESIAN_POINT('',(-0.5,12.,8.4));
#14169=CARTESIAN_POINT('Origin',(0.,12.,8.4));
#14170=CARTESIAN_POINT('Origin',(0.,12.,9.2));
#14171=CARTESIAN_POINT('Origin',(0.,12.,8.4));
#14172=CARTESIAN_POINT('',(0.,0.,0.));
#14173=CARTESIAN_POINT('Origin',(9.16515138991168,16.,8.4));
#14174=CARTESIAN_POINT('',(8.86015138991168,16.,9.2));
#14175=CARTESIAN_POINT('Origin',(9.16515138991168,16.,9.2));
#14176=CARTESIAN_POINT('',(8.86015138991168,16.,8.4));
#14177=CARTESIAN_POINT('',(8.86015138991168,16.,8.4));
#14178=CARTESIAN_POINT('Origin',(9.16515138991168,16.,8.4));
#14179=CARTESIAN_POINT('Origin',(9.16515138991168,16.,8.4));
#14180=CARTESIAN_POINT('',(8.66515138991168,16.,9.2));
#14181=CARTESIAN_POINT('Origin',(9.16515138991168,16.,9.2));
#14182=CARTESIAN_POINT('',(8.66515138991168,16.,8.4));
#14183=CARTESIAN_POINT('',(8.66515138991168,16.,8.4));
#14184=CARTESIAN_POINT('Origin',(9.16515138991168,16.,8.4));
#14185=CARTESIAN_POINT('Origin',(9.16515138991168,16.,9.2));
#14186=CARTESIAN_POINT('Origin',(9.16515138991168,16.,8.4));
#14187=CARTESIAN_POINT('',(0.,0.,0.));
#14188=CARTESIAN_POINT('',(0.,0.,0.));
#14189=CARTESIAN_POINT('',(0.,0.,0.));
#14190=CARTESIAN_POINT('',(0.,0.,0.));
#14191=CARTESIAN_POINT('',(0.,0.,0.));
#14192=CARTESIAN_POINT('Origin',(9.16515138991168,16.,3.3));
#14193=CARTESIAN_POINT('',(8.91515138991168,16.,3.4));
#14194=CARTESIAN_POINT('Origin',(9.16515138991168,16.,3.4));
#14195=CARTESIAN_POINT('',(8.91515138991168,16.,4.2));
#14196=CARTESIAN_POINT('',(8.91515138991168,16.,3.3));
#14197=CARTESIAN_POINT('Origin',(9.16515138991168,16.,4.2));
#14198=CARTESIAN_POINT('Origin',(10.6651513899117,14.1,3.3));
#14199=CARTESIAN_POINT('',(10.3901513899117,14.1,3.4));
#14200=CARTESIAN_POINT('Origin',(10.6651513899117,14.1,3.4));
#14201=CARTESIAN_POINT('',(10.3901513899117,14.1,4.2));
#14202=CARTESIAN_POINT('',(10.3901513899117,14.1,3.3));
#14203=CARTESIAN_POINT('Origin',(10.6651513899117,14.1,4.2));
#14204=CARTESIAN_POINT('Origin',(7.66515138991168,17.9,3.3));
#14205=CARTESIAN_POINT('',(7.39015138991168,17.9,3.4));
#14206=CARTESIAN_POINT('Origin',(7.66515138991168,17.9,3.4));
#14207=CARTESIAN_POINT('',(7.39015138991168,17.9,4.2));
#14208=CARTESIAN_POINT('',(7.39015138991168,17.9,3.3));
#14209=CARTESIAN_POINT('Origin',(7.66515138991168,17.9,4.2));
#14210=CARTESIAN_POINT('Origin',(7.66515138991168,14.1,3.3));
#14211=CARTESIAN_POINT('',(7.39015138991168,14.1,3.4));
#14212=CARTESIAN_POINT('Origin',(7.66515138991168,14.1,3.4));
#14213=CARTESIAN_POINT('',(7.39015138991168,14.1,4.2));
#14214=CARTESIAN_POINT('',(7.39015138991168,14.1,3.3));
#14215=CARTESIAN_POINT('Origin',(7.66515138991168,14.1,4.2));
#14216=CARTESIAN_POINT('Origin',(10.6651513899117,17.9,3.3));
#14217=CARTESIAN_POINT('',(10.3901513899117,17.9,3.4));
#14218=CARTESIAN_POINT('Origin',(10.6651513899117,17.9,3.4));
#14219=CARTESIAN_POINT('',(10.3901513899117,17.9,4.2));
#14220=CARTESIAN_POINT('',(10.3901513899117,17.9,3.3));
#14221=CARTESIAN_POINT('Origin',(10.6651513899117,17.9,4.2));
#14222=CARTESIAN_POINT('Origin',(12.6651513899117,19.,3.4));
#14223=CARTESIAN_POINT('',(12.6651513899117,19.,3.4));
#14224=CARTESIAN_POINT('',(5.66515138991168,19.,3.4));
#14225=CARTESIAN_POINT('',(12.6651513899117,19.,3.4));
#14226=CARTESIAN_POINT('',(5.66515138991168,19.,4.2));
#14227=CARTESIAN_POINT('',(5.66515138991168,19.,3.4));
#14228=CARTESIAN_POINT('',(12.6651513899117,19.,4.2));
#14229=CARTESIAN_POINT('',(12.6651513899117,19.,4.2));
#14230=CARTESIAN_POINT('',(12.6651513899117,19.,3.4));
#14231=CARTESIAN_POINT('Origin',(12.6651513899117,13.,3.4));
#14232=CARTESIAN_POINT('',(12.6651513899117,13.,3.4));
#14233=CARTESIAN_POINT('',(12.6651513899117,13.,3.4));
#14234=CARTESIAN_POINT('',(12.6651513899117,13.,4.2));
#14235=CARTESIAN_POINT('',(12.6651513899117,13.,4.2));
#14236=CARTESIAN_POINT('',(12.6651513899117,13.,3.4));
#14237=CARTESIAN_POINT('Origin',(5.66515138991168,13.,3.4));
#14238=CARTESIAN_POINT('',(5.66515138991168,13.,3.4));
#14239=CARTESIAN_POINT('',(5.66515138991168,13.,3.4));
#14240=CARTESIAN_POINT('',(5.66515138991168,13.,4.2));
#14241=CARTESIAN_POINT('',(5.66515138991168,13.,4.2));
#14242=CARTESIAN_POINT('',(5.66515138991168,13.,3.4));
#14243=CARTESIAN_POINT('Origin',(5.66515138991168,19.,3.4));
#14244=CARTESIAN_POINT('',(5.66515138991168,19.,3.4));
#14245=CARTESIAN_POINT('',(5.66515138991168,19.,4.2));
#14246=CARTESIAN_POINT('Origin',(9.16515138991168,16.,4.2));
#14247=CARTESIAN_POINT('Origin',(9.16515138991168,16.,3.4));
#14248=CARTESIAN_POINT('',(0.,0.,0.));
#14249=CARTESIAN_POINT('Origin',(9.16515138991168,16.,8.9));
#14250=CARTESIAN_POINT('',(9.00015138991168,16.,8.9));
#14251=CARTESIAN_POINT('Origin',(9.16515138991168,16.,8.9));
#14252=CARTESIAN_POINT('',(9.00015138991168,16.,9.8));
#14253=CARTESIAN_POINT('',(9.00015138991168,16.,8.9));
#14254=CARTESIAN_POINT('Origin',(9.16515138991168,16.,9.8));
#14255=CARTESIAN_POINT('Origin',(9.16515138991168,16.,8.9));
#14256=CARTESIAN_POINT('Origin',(9.16515138991168,16.,4.6));
#14257=CARTESIAN_POINT('',(8.46515138991168,16.,4.6));
#14258=CARTESIAN_POINT('Origin',(9.16515138991168,16.,4.6));
#14259=CARTESIAN_POINT('',(8.86515138991168,16.,4.6));
#14260=CARTESIAN_POINT('Origin',(9.16515138991168,16.,4.6));
#14261=CARTESIAN_POINT('Origin',(9.16515138991168,16.,4.2));
#14262=CARTESIAN_POINT('',(8.46515138991168,16.,4.2));
#14263=CARTESIAN_POINT('Origin',(9.16515138991168,16.,4.2));
#14264=CARTESIAN_POINT('',(8.86515138991168,16.,4.2));
#14265=CARTESIAN_POINT('Origin',(9.16515138991168,16.,4.2));
#14266=CARTESIAN_POINT('Origin',(9.16515138991168,16.,4.2));
#14267=CARTESIAN_POINT('',(8.46515138991168,16.,4.2));
#14268=CARTESIAN_POINT('Origin',(9.16515138991168,16.,3.4));
#14269=CARTESIAN_POINT('',(8.86515138991168,16.,3.4));
#14270=CARTESIAN_POINT('',(8.86515138991168,16.,3.4));
#14271=CARTESIAN_POINT('Origin',(9.16515138991168,16.,3.4));
#14272=CARTESIAN_POINT('Origin',(9.16515138991168,16.,3.4));
#14273=CARTESIAN_POINT('',(8.86515138991168,16.,9.8));
#14274=CARTESIAN_POINT('Origin',(9.16515138991168,16.,9.8));
#14275=CARTESIAN_POINT('',(8.86515138991168,16.,3.4));
#14276=CARTESIAN_POINT('Origin',(9.16515138991168,16.,9.8));
#14277=CARTESIAN_POINT('Origin',(9.16515138991168,16.,3.4));
#14278=CARTESIAN_POINT('',(0.,0.,0.));
#14279=CARTESIAN_POINT('Origin',(9.16515138991168,16.,4.6));
#14280=CARTESIAN_POINT('',(8.86015138991168,16.,8.4));
#14281=CARTESIAN_POINT('Origin',(9.16515138991168,16.,8.4));
#14282=CARTESIAN_POINT('',(8.86015138991168,16.,4.6));
#14283=CARTESIAN_POINT('',(8.86015138991168,16.,4.6));
#14284=CARTESIAN_POINT('Origin',(9.16515138991168,16.,4.6));
#14285=CARTESIAN_POINT('Origin',(9.16515138991168,16.,4.6));
#14286=CARTESIAN_POINT('',(8.66515138991168,16.,8.4));
#14287=CARTESIAN_POINT('Origin',(9.16515138991168,16.,8.4));
#14288=CARTESIAN_POINT('',(8.66515138991168,16.,4.6));
#14289=CARTESIAN_POINT('',(8.66515138991168,16.,4.6));
#14290=CARTESIAN_POINT('Origin',(9.16515138991168,16.,4.6));
#14291=CARTESIAN_POINT('Origin',(9.16515138991168,16.,8.4));
#14292=CARTESIAN_POINT('Origin',(9.16515138991168,16.,4.6));
#14293=CARTESIAN_POINT('',(0.,0.,0.));
#14294=CARTESIAN_POINT('Origin',(9.16515138991168,16.,9.2));
#14295=CARTESIAN_POINT('',(8.86015138991168,16.,9.8));
#14296=CARTESIAN_POINT('Origin',(9.16515138991168,16.,9.8));
#14297=CARTESIAN_POINT('',(8.86015138991168,16.,9.2));
#14298=CARTESIAN_POINT('',(8.86015138991168,16.,9.2));
#14299=CARTESIAN_POINT('Origin',(9.16515138991168,16.,9.2));
#14300=CARTESIAN_POINT('Origin',(9.16515138991168,16.,9.2));
#14301=CARTESIAN_POINT('',(8.66515138991168,16.,9.8));
#14302=CARTESIAN_POINT('Origin',(9.16515138991168,16.,9.8));
#14303=CARTESIAN_POINT('',(8.66515138991168,16.,9.2));
#14304=CARTESIAN_POINT('',(8.66515138991168,16.,9.2));
#14305=CARTESIAN_POINT('Origin',(9.16515138991168,16.,9.2));
#14306=CARTESIAN_POINT('Origin',(9.16515138991168,16.,9.8));
#14307=CARTESIAN_POINT('Origin',(9.16515138991168,16.,9.2));
#14308=CARTESIAN_POINT('',(0.,0.,0.));
#14309=CARTESIAN_POINT('Origin',(9.16515138991168,16.,9.8));
#14310=CARTESIAN_POINT('',(8.94015138991168,16.,10.));
#14311=CARTESIAN_POINT('Origin',(9.16515138991168,16.,10.));
#14312=CARTESIAN_POINT('',(8.94015138991168,16.,9.8));
#14313=CARTESIAN_POINT('',(8.94015138991168,16.,9.8));
#14314=CARTESIAN_POINT('Origin',(9.16515138991168,16.,9.8));
#14315=CARTESIAN_POINT('Origin',(9.16515138991168,16.,9.8));
#14316=CARTESIAN_POINT('',(8.66515138991168,16.,10.));
#14317=CARTESIAN_POINT('Origin',(9.16515138991168,16.,10.));
#14318=CARTESIAN_POINT('',(8.66515138991168,16.,9.8));
#14319=CARTESIAN_POINT('',(8.66515138991168,16.,9.8));
#14320=CARTESIAN_POINT('Origin',(9.16515138991168,16.,9.8));
#14321=CARTESIAN_POINT('Origin',(9.16515138991168,16.,10.));
#14322=CARTESIAN_POINT('Origin',(9.16515138991168,16.,9.8));
#14323=CARTESIAN_POINT('',(0.,0.,0.));
#14324=CARTESIAN_POINT('',(0.,0.,0.));
#14325=CARTESIAN_POINT('Origin',(1.5,-1.9,1.7));
#14326=CARTESIAN_POINT('',(1.56403124237433,-1.7,1.7));
#14327=CARTESIAN_POINT('',(1.43596875762567,-1.7,1.7));
#14328=CARTESIAN_POINT('',(0.75,-1.7,1.7));
#14329=CARTESIAN_POINT('Origin',(1.5,-1.9,1.7));
#14330=CARTESIAN_POINT('Origin',(1.5,-1.9,1.7));
#14331=CARTESIAN_POINT('',(1.56403124237433,-1.7,1.75));
#14332=CARTESIAN_POINT('',(1.56403124237433,-1.7,1.7));
#14333=CARTESIAN_POINT('',(1.29,-1.9,1.75));
#14334=CARTESIAN_POINT('Origin',(1.5,-1.9,1.75));
#14335=CARTESIAN_POINT('',(1.29,-1.9,2.4));
#14336=CARTESIAN_POINT('',(1.29,-1.9,1.7));
#14337=CARTESIAN_POINT('Origin',(1.5,-1.9,2.4));
#14338=CARTESIAN_POINT('',(1.43596875762567,-1.7,1.75));
#14339=CARTESIAN_POINT('Origin',(1.5,-1.9,1.75));
#14340=CARTESIAN_POINT('',(1.43596875762567,-1.7,1.7));
#14341=CARTESIAN_POINT('Origin',(-1.5,1.9,1.7));
#14342=CARTESIAN_POINT('',(-1.56403124237433,1.7,1.7));
#14343=CARTESIAN_POINT('',(-1.43596875762567,1.7,1.7));
#14344=CARTESIAN_POINT('',(-0.75,1.7,1.7));
#14345=CARTESIAN_POINT('Origin',(-1.5,1.9,1.7));
#14346=CARTESIAN_POINT('Origin',(-1.5,1.9,1.7));
#14347=CARTESIAN_POINT('',(-1.56403124237433,1.7,1.75));
#14348=CARTESIAN_POINT('',(-1.56403124237433,1.7,1.7));
#14349=CARTESIAN_POINT('',(-1.71,1.9,1.75));
#14350=CARTESIAN_POINT('Origin',(-1.5,1.9,1.75));
#14351=CARTESIAN_POINT('',(-1.71,1.9,2.4));
#14352=CARTESIAN_POINT('',(-1.71,1.9,1.7));
#14353=CARTESIAN_POINT('Origin',(-1.5,1.9,2.4));
#14354=CARTESIAN_POINT('',(-1.43596875762567,1.7,1.75));
#14355=CARTESIAN_POINT('Origin',(-1.5,1.9,1.75));
#14356=CARTESIAN_POINT('',(-1.43596875762567,1.7,1.7));
#14357=CARTESIAN_POINT('Origin',(-1.5,-1.9,1.7));
#14358=CARTESIAN_POINT('',(-1.43596875762567,-1.7,1.7));
#14359=CARTESIAN_POINT('',(-1.56403124237433,-1.7,1.7));
#14360=CARTESIAN_POINT('',(-0.75,-1.7,1.7));
#14361=CARTESIAN_POINT('Origin',(-1.5,-1.9,1.7));
#14362=CARTESIAN_POINT('Origin',(-1.5,-1.9,1.7));
#14363=CARTESIAN_POINT('',(-1.43596875762567,-1.7,1.75));
#14364=CARTESIAN_POINT('',(-1.43596875762567,-1.7,1.7));
#14365=CARTESIAN_POINT('',(-1.71,-1.9,1.75));
#14366=CARTESIAN_POINT('Origin',(-1.5,-1.9,1.75));
#14367=CARTESIAN_POINT('',(-1.71,-1.9,2.4));
#14368=CARTESIAN_POINT('',(-1.71,-1.9,1.7));
#14369=CARTESIAN_POINT('Origin',(-1.5,-1.9,2.4));
#14370=CARTESIAN_POINT('',(-1.56403124237433,-1.7,1.75));
#14371=CARTESIAN_POINT('Origin',(-1.5,-1.9,1.75));
#14372=CARTESIAN_POINT('',(-1.56403124237433,-1.7,1.7));
#14373=CARTESIAN_POINT('Origin',(1.5,1.9,1.7));
#14374=CARTESIAN_POINT('',(1.43596875762567,1.7,1.7));
#14375=CARTESIAN_POINT('',(1.56403124237433,1.7,1.7));
#14376=CARTESIAN_POINT('',(0.75,1.7,1.7));
#14377=CARTESIAN_POINT('Origin',(1.5,1.9,1.7));
#14378=CARTESIAN_POINT('Origin',(1.5,1.9,1.7));
#14379=CARTESIAN_POINT('',(1.43596875762567,1.7,1.75));
#14380=CARTESIAN_POINT('',(1.43596875762567,1.7,1.7));
#14381=CARTESIAN_POINT('',(1.29,1.9,1.75));
#14382=CARTESIAN_POINT('Origin',(1.5,1.9,1.75));
#14383=CARTESIAN_POINT('',(1.29,1.9,2.4));
#14384=CARTESIAN_POINT('',(1.29,1.9,1.7));
#14385=CARTESIAN_POINT('Origin',(1.5,1.9,2.4));
#14386=CARTESIAN_POINT('',(1.56403124237433,1.7,1.75));
#14387=CARTESIAN_POINT('Origin',(1.5,1.9,1.75));
#14388=CARTESIAN_POINT('',(1.56403124237433,1.7,1.7));
#14389=CARTESIAN_POINT('Origin',(0.,-1.7,1.75));
#14390=CARTESIAN_POINT('',(0.,-1.7,1.75));
#14391=CARTESIAN_POINT('',(-1.97,-1.7,1.75));
#14392=CARTESIAN_POINT('',(0.,-1.7,1.75));
#14393=CARTESIAN_POINT('',(-1.97,-1.7,0.43));
#14394=CARTESIAN_POINT('',(-1.97,-1.7,1.75));
#14395=CARTESIAN_POINT('',(1.97,-1.7,0.43));
#14396=CARTESIAN_POINT('',(0.,-1.7,0.43));
#14397=CARTESIAN_POINT('',(1.97,-1.7,1.75));
#14398=CARTESIAN_POINT('',(1.97,-1.7,1.75));
#14399=CARTESIAN_POINT('',(0.,-1.7,1.75));
#14400=CARTESIAN_POINT('Origin',(0.,1.7,0.43));
#14401=CARTESIAN_POINT('',(0.,1.7,1.75));
#14402=CARTESIAN_POINT('',(1.97,1.7,1.75));
#14403=CARTESIAN_POINT('',(0.,1.7,1.75));
#14404=CARTESIAN_POINT('',(1.97,1.7,0.43));
#14405=CARTESIAN_POINT('',(1.97,1.7,0.43));
#14406=CARTESIAN_POINT('',(-1.97,1.7,0.43));
#14407=CARTESIAN_POINT('',(0.,1.7,0.43));
#14408=CARTESIAN_POINT('',(-1.97,1.7,1.75));
#14409=CARTESIAN_POINT('',(-1.97,1.7,0.43));
#14410=CARTESIAN_POINT('',(0.,1.7,1.75));
#14411=CARTESIAN_POINT('Origin',(-1.97,0.,1.415));
#14412=CARTESIAN_POINT('',(-1.97,-2.35,1.75));
#14413=CARTESIAN_POINT('',(-1.97,-2.35,1.75));
#14414=CARTESIAN_POINT('',(-1.97,-2.35,2.4));
#14415=CARTESIAN_POINT('',(-1.97,-2.35,2.4));
#14416=CARTESIAN_POINT('',(-1.97,2.35,2.4));
#14417=CARTESIAN_POINT('',(-1.97,2.35,2.4));
#14418=CARTESIAN_POINT('',(-1.97,2.35,1.75));
#14419=CARTESIAN_POINT('',(-1.97,2.35,1.75));
#14420=CARTESIAN_POINT('',(-1.97,1.7,1.75));
#14421=CARTESIAN_POINT('',(-1.97,0.78,0.43));
#14422=CARTESIAN_POINT('',(-1.97,0.78,0.43));
#14423=CARTESIAN_POINT('',(-1.97,0.78,1.55));
#14424=CARTESIAN_POINT('',(-1.97,0.78,1.55));
#14425=CARTESIAN_POINT('',(-1.97,-0.78,1.55));
#14426=CARTESIAN_POINT('',(-1.97,-0.78,1.55));
#14427=CARTESIAN_POINT('',(-1.97,-0.78,0.43));
#14428=CARTESIAN_POINT('',(-1.97,-0.78,0.43));
#14429=CARTESIAN_POINT('',(-1.97,-1.7,0.43));
#14430=CARTESIAN_POINT('Origin',(0.,-2.35,1.75));
#14431=CARTESIAN_POINT('',(1.97,-2.35,1.75));
#14432=CARTESIAN_POINT('',(1.97,-2.35,1.75));
#14433=CARTESIAN_POINT('',(0.,-2.35,1.75));
#14434=CARTESIAN_POINT('Origin',(0.,-2.35,2.4));
#14435=CARTESIAN_POINT('',(1.97,-2.35,2.4));
#14436=CARTESIAN_POINT('',(1.97,-2.35,2.4));
#14437=CARTESIAN_POINT('',(0.,-2.35,2.4));
#14438=CARTESIAN_POINT('Origin',(0.,2.35,2.4));
#14439=CARTESIAN_POINT('',(1.97,2.35,2.4));
#14440=CARTESIAN_POINT('',(1.97,2.35,2.4));
#14441=CARTESIAN_POINT('',(0.,2.35,2.4));
#14442=CARTESIAN_POINT('Origin',(0.,2.35,1.75));
#14443=CARTESIAN_POINT('',(1.97,2.35,1.75));
#14444=CARTESIAN_POINT('',(1.97,2.35,1.75));
#14445=CARTESIAN_POINT('',(0.,2.35,1.75));
#14446=CARTESIAN_POINT('Origin',(0.,1.7,1.75));
#14447=CARTESIAN_POINT('',(1.97,1.7,1.75));
#14448=CARTESIAN_POINT('Origin',(0.,0.78,0.43));
#14449=CARTESIAN_POINT('',(1.97,0.78,0.43));
#14450=CARTESIAN_POINT('',(1.97,0.78,0.43));
#14451=CARTESIAN_POINT('',(0.,0.78,0.43));
#14452=CARTESIAN_POINT('Origin',(0.,0.78,1.55));
#14453=CARTESIAN_POINT('',(1.97,0.78,1.55));
#14454=CARTESIAN_POINT('',(1.97,0.78,1.55));
#14455=CARTESIAN_POINT('',(0.,0.78,1.55));
#14456=CARTESIAN_POINT('Origin',(0.,-0.78,1.55));
#14457=CARTESIAN_POINT('',(1.97,-0.78,1.55));
#14458=CARTESIAN_POINT('',(1.97,-0.78,1.55));
#14459=CARTESIAN_POINT('',(0.,-0.78,1.55));
#14460=CARTESIAN_POINT('Origin',(0.,-0.78,0.43));
#14461=CARTESIAN_POINT('',(1.97,-0.78,0.43));
#14462=CARTESIAN_POINT('',(1.97,-0.78,0.43));
#14463=CARTESIAN_POINT('',(0.,-0.78,0.43));
#14464=CARTESIAN_POINT('Origin',(0.,-1.7,0.43));
#14465=CARTESIAN_POINT('',(1.97,-1.7,0.43));
#14466=CARTESIAN_POINT('Origin',(1.97,0.,1.415));
#14467=CARTESIAN_POINT('',(0.,0.,0.));
#14468=CARTESIAN_POINT('Origin',(1.97,1.7,2.3));
#14469=CARTESIAN_POINT('',(1.97,1.7,2.3));
#14470=CARTESIAN_POINT('',(1.97,-1.7,2.3));
#14471=CARTESIAN_POINT('',(1.97,1.7,2.3));
#14472=CARTESIAN_POINT('',(3.07,-1.7,2.3));
#14473=CARTESIAN_POINT('',(1.97,-1.7,2.3));
#14474=CARTESIAN_POINT('',(3.07,1.7,2.3));
#14475=CARTESIAN_POINT('',(3.07,1.7,2.3));
#14476=CARTESIAN_POINT('',(1.97,1.7,2.3));
#14477=CARTESIAN_POINT('Origin',(1.97,1.7,0.46));
#14478=CARTESIAN_POINT('',(1.97,1.7,0.46));
#14479=CARTESIAN_POINT('',(1.97,1.7,0.46));
#14480=CARTESIAN_POINT('',(3.07,1.7,0.46));
#14481=CARTESIAN_POINT('',(3.07,1.7,0.46));
#14482=CARTESIAN_POINT('',(1.97,1.7,0.46));
#14483=CARTESIAN_POINT('Origin',(1.97,0.78,0.46));
#14484=CARTESIAN_POINT('',(1.97,0.78,0.46));
#14485=CARTESIAN_POINT('',(1.97,0.78,0.46));
#14486=CARTESIAN_POINT('',(3.07,0.78,0.46));
#14487=CARTESIAN_POINT('',(3.07,0.78,0.46));
#14488=CARTESIAN_POINT('',(1.97,0.78,0.46));
#14489=CARTESIAN_POINT('Origin',(1.97,0.78,1.55));
#14490=CARTESIAN_POINT('',(1.97,0.78,1.55));
#14491=CARTESIAN_POINT('',(1.97,0.78,1.55));
#14492=CARTESIAN_POINT('',(3.07,0.78,1.55));
#14493=CARTESIAN_POINT('',(3.07,0.78,1.55));
#14494=CARTESIAN_POINT('',(1.97,0.78,1.55));
#14495=CARTESIAN_POINT('Origin',(1.97,-0.78,1.55));
#14496=CARTESIAN_POINT('',(1.97,-0.78,1.55));
#14497=CARTESIAN_POINT('',(1.97,-0.78,1.55));
#14498=CARTESIAN_POINT('',(3.07,-0.78,1.55));
#14499=CARTESIAN_POINT('',(3.07,-0.78,1.55));
#14500=CARTESIAN_POINT('',(1.97,-0.78,1.55));
#14501=CARTESIAN_POINT('Origin',(1.97,-0.78,0.46));
#14502=CARTESIAN_POINT('',(1.97,-0.78,0.46));
#14503=CARTESIAN_POINT('',(1.97,-0.78,0.46));
#14504=CARTESIAN_POINT('',(3.07,-0.78,0.46));
#14505=CARTESIAN_POINT('',(3.07,-0.78,0.46));
#14506=CARTESIAN_POINT('',(1.97,-0.78,0.46));
#14507=CARTESIAN_POINT('Origin',(1.97,-1.7,0.46));
#14508=CARTESIAN_POINT('',(1.97,-1.7,0.46));
#14509=CARTESIAN_POINT('',(1.97,-1.7,0.46));
#14510=CARTESIAN_POINT('',(3.07,-1.7,0.46));
#14511=CARTESIAN_POINT('',(3.07,-1.7,0.46));
#14512=CARTESIAN_POINT('',(1.97,-1.7,0.46));
#14513=CARTESIAN_POINT('Origin',(1.97,-1.7,2.3));
#14514=CARTESIAN_POINT('',(1.97,-1.7,2.3));
#14515=CARTESIAN_POINT('',(3.07,-1.7,2.3));
#14516=CARTESIAN_POINT('Origin',(3.07,0.,1.38));
#14517=CARTESIAN_POINT('Origin',(1.97,0.,1.38));
#14518=CARTESIAN_POINT('',(0.,0.,0.));
#14519=CARTESIAN_POINT('Origin',(-1.97,-0.78,0.46));
#14520=CARTESIAN_POINT('',(-1.97,-1.7,0.46));
#14521=CARTESIAN_POINT('',(-1.97,-0.78,0.46));
#14522=CARTESIAN_POINT('',(-1.97,-1.7,0.46));
#14523=CARTESIAN_POINT('',(-3.07,-1.7,0.46));
#14524=CARTESIAN_POINT('',(-1.97,-1.7,0.46));
#14525=CARTESIAN_POINT('',(-3.07,-0.78,0.46));
#14526=CARTESIAN_POINT('',(-3.07,-1.7,0.46));
#14527=CARTESIAN_POINT('',(-1.97,-0.78,0.46));
#14528=CARTESIAN_POINT('Origin',(-1.97,-0.78,1.55));
#14529=CARTESIAN_POINT('',(-1.97,-0.78,1.55));
#14530=CARTESIAN_POINT('',(-1.97,-0.78,0.46));
#14531=CARTESIAN_POINT('',(-3.07,-0.78,1.55));
#14532=CARTESIAN_POINT('',(-3.07,-0.78,0.46));
#14533=CARTESIAN_POINT('',(-1.97,-0.78,1.55));
#14534=CARTESIAN_POINT('Origin',(-1.97,0.78,1.55));
#14535=CARTESIAN_POINT('',(-1.97,0.78,1.55));
#14536=CARTESIAN_POINT('',(-1.97,-0.78,1.55));
#14537=CARTESIAN_POINT('',(-3.07,0.78,1.55));
#14538=CARTESIAN_POINT('',(-3.07,-0.78,1.55));
#14539=CARTESIAN_POINT('',(-1.97,0.78,1.55));
#14540=CARTESIAN_POINT('Origin',(-1.97,0.78,0.46));
#14541=CARTESIAN_POINT('',(-1.97,0.78,0.46));
#14542=CARTESIAN_POINT('',(-1.97,0.78,1.55));
#14543=CARTESIAN_POINT('',(-3.07,0.78,0.46));
#14544=CARTESIAN_POINT('',(-3.07,0.78,1.55));
#14545=CARTESIAN_POINT('',(-1.97,0.78,0.46));
#14546=CARTESIAN_POINT('Origin',(-1.97,1.7,0.46));
#14547=CARTESIAN_POINT('',(-1.97,1.7,0.46));
#14548=CARTESIAN_POINT('',(-1.97,0.78,0.46));
#14549=CARTESIAN_POINT('',(-3.07,1.7,0.46));
#14550=CARTESIAN_POINT('',(-3.07,0.78,0.46));
#14551=CARTESIAN_POINT('',(-1.97,1.7,0.46));
#14552=CARTESIAN_POINT('Origin',(-1.97,1.7,2.3));
#14553=CARTESIAN_POINT('',(-1.97,1.7,2.3));
#14554=CARTESIAN_POINT('',(-1.97,1.7,0.46));
#14555=CARTESIAN_POINT('',(-3.07,1.7,2.3));
#14556=CARTESIAN_POINT('',(-3.07,1.7,0.46));
#14557=CARTESIAN_POINT('',(-1.97,1.7,2.3));
#14558=CARTESIAN_POINT('Origin',(-1.97,-1.7,2.3));
#14559=CARTESIAN_POINT('',(-1.97,-1.7,2.3));
#14560=CARTESIAN_POINT('',(-1.97,1.7,2.3));
#14561=CARTESIAN_POINT('',(-3.07,-1.7,2.3));
#14562=CARTESIAN_POINT('',(-3.07,1.7,2.3));
#14563=CARTESIAN_POINT('',(-1.97,-1.7,2.3));
#14564=CARTESIAN_POINT('Origin',(-1.97,-1.7,0.46));
#14565=CARTESIAN_POINT('',(-1.97,-1.7,2.3));
#14566=CARTESIAN_POINT('',(-3.07,-1.7,2.3));
#14567=CARTESIAN_POINT('Origin',(-1.97,0.,1.38));
#14568=CARTESIAN_POINT('Origin',(-3.07,0.,1.38));
#14569=CARTESIAN_POINT('',(0.,0.,0.));
#14570=CARTESIAN_POINT('',(0.,0.,0.));
#14571=CARTESIAN_POINT('',(0.,0.,0.));
#14572=CARTESIAN_POINT('',(0.,0.,0.));
#14573=CARTESIAN_POINT('Origin',(0.115470053837925,-0.5,-0.2));
#14574=CARTESIAN_POINT('',(0.23094010767585,-0.5,0.));
#14575=CARTESIAN_POINT('',(0.115470053837925,-0.5,-0.2));
#14576=CARTESIAN_POINT('',(0.23094010767585,-0.5,0.));
#14577=CARTESIAN_POINT('',(0.115470053837925,-0.8,-0.2));
#14578=CARTESIAN_POINT('',(0.115470053837925,-0.5,-0.2));
#14579=CARTESIAN_POINT('',(0.23094010767585,-0.8,0.));
#14580=CARTESIAN_POINT('',(0.23094010767585,-0.8,0.));
#14581=CARTESIAN_POINT('',(0.23094010767585,-0.5,0.));
#14582=CARTESIAN_POINT('Origin',(-0.115470053837925,-0.5,-0.2));
#14583=CARTESIAN_POINT('',(-0.115470053837925,-0.5,-0.2));
#14584=CARTESIAN_POINT('',(0.115470053837925,-0.5,-0.2));
#14585=CARTESIAN_POINT('',(-0.115470053837925,-0.8,-0.2));
#14586=CARTESIAN_POINT('',(-0.115470053837925,-0.5,-0.2));
#14587=CARTESIAN_POINT('',(0.115470053837925,-0.8,-0.2));
#14588=CARTESIAN_POINT('Origin',(-0.23094010767585,-0.5,-2.77555756156289E-17));
#14589=CARTESIAN_POINT('',(-0.23094010767585,-0.5,-2.82820063659975E-17));
#14590=CARTESIAN_POINT('',(-0.115470053837925,-0.5,-0.2));
#14591=CARTESIAN_POINT('',(-0.23094010767585,-0.8,-2.77555756156289E-17));
#14592=CARTESIAN_POINT('',(-0.23094010767585,-0.5,-2.82820063659975E-17));
#14593=CARTESIAN_POINT('',(-0.115470053837925,-0.8,-0.2));
#14594=CARTESIAN_POINT('Origin',(-0.115470053837925,-0.5,0.2));
#14595=CARTESIAN_POINT('',(-0.115470053837925,-0.5,0.2));
#14596=CARTESIAN_POINT('',(-0.23094010767585,-0.5,-2.82820063659975E-17));
#14597=CARTESIAN_POINT('',(-0.115470053837925,-0.8,0.2));
#14598=CARTESIAN_POINT('',(-0.115470053837925,-0.5,0.2));
#14599=CARTESIAN_POINT('',(-0.23094010767585,-0.8,-2.82820063659975E-17));
#14600=CARTESIAN_POINT('Origin',(0.115470053837925,-0.5,0.2));
#14601=CARTESIAN_POINT('',(0.115470053837925,-0.5,0.2));
#14602=CARTESIAN_POINT('',(-0.115470053837925,-0.5,0.2));
#14603=CARTESIAN_POINT('',(0.115470053837925,-0.8,0.2));
#14604=CARTESIAN_POINT('',(0.115470053837925,-0.5,0.2));
#14605=CARTESIAN_POINT('',(-0.115470053837925,-0.8,0.2));
#14606=CARTESIAN_POINT('Origin',(0.23094010767585,-0.5,0.));
#14607=CARTESIAN_POINT('',(0.115470053837925,-0.5,0.2));
#14608=CARTESIAN_POINT('',(0.115470053837925,-0.8,0.2));
#14609=CARTESIAN_POINT('Origin',(0.,-0.5,0.));
#14610=CARTESIAN_POINT('Origin',(0.,-0.8,0.));
#14611=CARTESIAN_POINT('Origin',(0.,-1.4,0.));
#14612=CARTESIAN_POINT('',(-0.24505,-1.4,3.00099698131059E-17));
#14613=CARTESIAN_POINT('Origin',(0.,-1.4,0.));
#14614=CARTESIAN_POINT('Origin',(0.375,0.5,0.));
#14615=CARTESIAN_POINT('',(-0.375,0.5,-4.59242549680257E-17));
#14616=CARTESIAN_POINT('Origin',(0.,0.5,0.));
#14617=CARTESIAN_POINT('Origin',(0.,0.475,0.));
#14618=CARTESIAN_POINT('',(-0.425,0.45,-5.20474889637625E-17));
#14619=CARTESIAN_POINT('Origin',(0.,0.45,0.));
#14620=CARTESIAN_POINT('',(-0.4,0.475,-4.89858719658941E-17));
#14621=CARTESIAN_POINT('Origin',(0.,0.24,0.));
#14622=CARTESIAN_POINT('',(-0.425,0.0299999999999998,-5.20474889637625E-17));
#14623=CARTESIAN_POINT('Origin',(0.,0.0299999999999998,0.));
#14624=CARTESIAN_POINT('',(-0.425,0.24,-5.20474889637625E-17));
#14625=CARTESIAN_POINT('Origin',(0.,0.0150000000000001,0.));
#14626=CARTESIAN_POINT('',(-0.395,4.85722573273506E-17,-4.83735485663204E-17));
#14627=CARTESIAN_POINT('Origin',(0.,0.,0.));
#14628=CARTESIAN_POINT('',(-0.41,0.0150000000000001,-5.02105187650415E-17));
#14629=CARTESIAN_POINT('Origin',(0.27,0.,0.));
#14630=CARTESIAN_POINT('',(-0.27,0.,-3.30654635769785E-17));
#14631=CARTESIAN_POINT('Origin',(0.,0.,0.));
#14632=CARTESIAN_POINT('Origin',(0.,-0.02,0.));
#14633=CARTESIAN_POINT('',(-0.24505,-0.0498999999999999,3.00099698131059E-17));
#14634=CARTESIAN_POINT('Origin',(0.,-0.0498999999999999,0.));
#14635=CARTESIAN_POINT('',(-0.26,-0.02,-3.18408167778312E-17));
#14636=CARTESIAN_POINT('Origin',(0.,-0.995,0.));
#14637=CARTESIAN_POINT('',(-0.24505,-0.995,-3.00099698131059E-17));
#14638=CARTESIAN_POINT('',(0.,0.,0.));
#14639=CARTESIAN_POINT('Origin',(0.0866025403784439,-0.4,-0.15));
#14640=CARTESIAN_POINT('',(0.173205080756888,-0.4,0.));
#14641=CARTESIAN_POINT('',(0.0866025403784439,-0.4,-0.15));
#14642=CARTESIAN_POINT('',(0.173205080756888,-0.4,0.));
#14643=CARTESIAN_POINT('',(0.0866025403784439,-0.64,-0.15));
#14644=CARTESIAN_POINT('',(0.0866025403784439,-0.4,-0.15));
#14645=CARTESIAN_POINT('',(0.173205080756888,-0.64,0.));
#14646=CARTESIAN_POINT('',(0.173205080756888,-0.64,0.));
#14647=CARTESIAN_POINT('',(0.173205080756888,-0.4,0.));
#14648=CARTESIAN_POINT('Origin',(-0.0866025403784438,-0.4,-0.15));
#14649=CARTESIAN_POINT('',(-0.0866025403784438,-0.4,-0.15));
#14650=CARTESIAN_POINT('',(0.0866025403784439,-0.4,-0.15));
#14651=CARTESIAN_POINT('',(-0.0866025403784438,-0.64,-0.15));
#14652=CARTESIAN_POINT('',(-0.0866025403784438,-0.4,-0.15));
#14653=CARTESIAN_POINT('',(0.0866025403784439,-0.64,-0.15));
#14654=CARTESIAN_POINT('Origin',(-0.173205080756888,-0.4,-2.77555756156289E-17));
#14655=CARTESIAN_POINT('',(-0.173205080756888,-0.4,-2.12115047744981E-17));
#14656=CARTESIAN_POINT('',(-0.0866025403784438,-0.4,-0.15));
#14657=CARTESIAN_POINT('',(-0.173205080756888,-0.64,-2.77555756156289E-17));
#14658=CARTESIAN_POINT('',(-0.173205080756888,-0.4,-2.12115047744981E-17));
#14659=CARTESIAN_POINT('',(-0.0866025403784438,-0.64,-0.15));
#14660=CARTESIAN_POINT('Origin',(-0.0866025403784439,-0.4,0.15));
#14661=CARTESIAN_POINT('',(-0.0866025403784439,-0.4,0.15));
#14662=CARTESIAN_POINT('',(-0.173205080756888,-0.4,-2.12115047744981E-17));
#14663=CARTESIAN_POINT('',(-0.0866025403784439,-0.64,0.15));
#14664=CARTESIAN_POINT('',(-0.0866025403784439,-0.4,0.15));
#14665=CARTESIAN_POINT('',(-0.173205080756888,-0.64,-2.12115047744981E-17));
#14666=CARTESIAN_POINT('Origin',(0.0866025403784439,-0.4,0.15));
#14667=CARTESIAN_POINT('',(0.0866025403784439,-0.4,0.15));
#14668=CARTESIAN_POINT('',(-0.0866025403784439,-0.4,0.15));
#14669=CARTESIAN_POINT('',(0.0866025403784439,-0.64,0.15));
#14670=CARTESIAN_POINT('',(0.0866025403784439,-0.4,0.15));
#14671=CARTESIAN_POINT('',(-0.0866025403784439,-0.64,0.15));
#14672=CARTESIAN_POINT('Origin',(0.173205080756888,-0.4,0.));
#14673=CARTESIAN_POINT('',(0.0866025403784439,-0.4,0.15));
#14674=CARTESIAN_POINT('',(0.0866025403784439,-0.64,0.15));
#14675=CARTESIAN_POINT('Origin',(0.,-0.4,-2.77555756156289E-17));
#14676=CARTESIAN_POINT('Origin',(0.,-0.64,-2.77555756156289E-17));
#14677=CARTESIAN_POINT('Origin',(0.,-1.,0.));
#14678=CARTESIAN_POINT('',(-0.1954,-1.,2.39295984553393E-17));
#14679=CARTESIAN_POINT('Origin',(0.,-1.,0.));
#14680=CARTESIAN_POINT('Origin',(0.3,0.4,0.));
#14681=CARTESIAN_POINT('',(-0.3,0.4,-3.67394039744206E-17));
#14682=CARTESIAN_POINT('Origin',(0.,0.4,0.));
#14683=CARTESIAN_POINT('Origin',(0.,0.375,0.));
#14684=CARTESIAN_POINT('',(-0.35,0.35,-4.28626379701573E-17));
#14685=CARTESIAN_POINT('Origin',(0.,0.35,0.));
#14686=CARTESIAN_POINT('',(-0.325,0.375,-3.9801020972289E-17));
#14687=CARTESIAN_POINT('Origin',(0.,0.19,0.));
#14688=CARTESIAN_POINT('',(-0.35,0.03,-4.28626379701574E-17));
#14689=CARTESIAN_POINT('Origin',(0.,0.03,0.));
#14690=CARTESIAN_POINT('',(-0.35,0.19,-4.28626379701574E-17));
#14691=CARTESIAN_POINT('Origin',(0.,0.0149999999999999,0.));
#14692=CARTESIAN_POINT('',(-0.32,-3.29597460435593E-17,-3.91886975727153E-17));
#14693=CARTESIAN_POINT('Origin',(0.,0.,0.));
#14694=CARTESIAN_POINT('',(-0.335,0.0149999999999999,-4.10256677714363E-17));
#14695=CARTESIAN_POINT('Origin',(0.22,0.,0.));
#14696=CARTESIAN_POINT('',(-0.22,-6.93889390390723E-18,-2.69422295812418E-17));
#14697=CARTESIAN_POINT('Origin',(0.,0.,0.));
#14698=CARTESIAN_POINT('Origin',(0.,-0.02,0.));
#14699=CARTESIAN_POINT('',(-0.1954,-0.0492,2.39295984553393E-17));
#14700=CARTESIAN_POINT('Origin',(0.,-0.0492,0.));
#14701=CARTESIAN_POINT('',(-0.21,-0.02,-2.57175827820944E-17));
#14702=CARTESIAN_POINT('Origin',(0.,-0.8,0.));
#14703=CARTESIAN_POINT('',(-0.1954,-0.8,-2.39295984553393E-17));
#14704=CARTESIAN_POINT('',(0.,0.,0.));
#14705=CARTESIAN_POINT('',(0.,0.,0.));
#14706=CARTESIAN_POINT('',(0.,0.,0.));
#14707=CARTESIAN_POINT('',(0.,0.,0.));
#14708=CARTESIAN_POINT('',(0.,0.,0.));
#14709=CARTESIAN_POINT('',(0.,0.,0.));
#14710=CARTESIAN_POINT('',(0.,0.,0.));
#14711=CARTESIAN_POINT('',(-1.5,16.,1.));
#14712=CARTESIAN_POINT('',(0.5,16.,1.97));
#14713=CARTESIAN_POINT('',(6.5,16.,1.97));
#14714=CARTESIAN_POINT('',(12.5,16.,1.97));
#14715=CARTESIAN_POINT('',(18.5,16.,1.97));
#14716=CARTESIAN_POINT('',(1.69705627484771,1.69705627484772,1.8));
#14717=CARTESIAN_POINT('',(-1.69705627484771,1.69705627484771,1.8));
#14718=CARTESIAN_POINT('',(-1.69705627484771,-1.69705627484771,1.8));
#14719=CARTESIAN_POINT('',(1.69705627484771,-1.69705627484771,1.8));
#14720=CARTESIAN_POINT('',(0.,0.,2.5));
#14721=CARTESIAN_POINT('',(1.23743686707646,1.23743686707646,4.));
#14722=CARTESIAN_POINT('',(-1.23743686707646,1.23743686707646,4.));
#14723=CARTESIAN_POINT('',(-1.23743686707646,-1.23743686707646,4.));
#14724=CARTESIAN_POINT('',(1.23743686707646,-1.23743686707646,4.));
#14725=CARTESIAN_POINT('',(1.69705627484771,7.69705627484771,1.8));
#14726=CARTESIAN_POINT('',(-1.69705627484771,7.69705627484771,1.8));
#14727=CARTESIAN_POINT('',(-1.69705627484771,4.30294372515229,1.8));
#14728=CARTESIAN_POINT('',(1.69705627484771,4.30294372515229,1.8));
#14729=CARTESIAN_POINT('',(0.,6.,2.5));
#14730=CARTESIAN_POINT('',(1.23743686707646,7.23743686707646,4.));
#14731=CARTESIAN_POINT('',(-1.23743686707646,7.23743686707646,4.));
#14732=CARTESIAN_POINT('',(-1.23743686707646,4.76256313292354,4.));
#14733=CARTESIAN_POINT('',(1.23743686707646,4.76256313292354,4.));
#14734=CARTESIAN_POINT('',(0.,0.,0.));
#14735=CARTESIAN_POINT('',(0.,0.,0.));
#14736=CARTESIAN_POINT('',(0.,0.,0.));
#14737=CARTESIAN_POINT('',(0.,0.,0.));
#14738=CARTESIAN_POINT('',(0.,0.,0.));
#14739=CARTESIAN_POINT('',(0.,0.,0.));
#14740=CARTESIAN_POINT('',(0.,0.,0.));
#14741=CARTESIAN_POINT('',(0.,0.,0.));
#14742=CARTESIAN_POINT('',(-3.2,6.,5.6));
#14743=CARTESIAN_POINT('',(0.9,6.,1.4));
#14744=CARTESIAN_POINT('',(0.,9.,8.2));
#14745=CARTESIAN_POINT('',(0.,0.,0.));
#14746=CARTESIAN_POINT('',(0.,0.,0.));
#14747=CARTESIAN_POINT('',(0.,0.,0.));
#14748=CARTESIAN_POINT('',(0.,0.,0.));
#14749=CARTESIAN_POINT('',(0.,0.,0.));
#14750=CARTESIAN_POINT('',(0.,0.,0.));
#14751=CARTESIAN_POINT('',(0.,0.,0.));
#14752=CARTESIAN_POINT('',(0.9,0.,1.4));
#14753=CARTESIAN_POINT('',(0.,12.,10.));
#14754=CARTESIAN_POINT('',(0.,0.,0.));
#14755=CARTESIAN_POINT('',(0.,0.,0.));
#14756=CARTESIAN_POINT('',(0.,0.,0.));
#14757=CARTESIAN_POINT('',(0.,0.,0.));
#14758=CARTESIAN_POINT('',(0.,0.,0.));
#14759=CARTESIAN_POINT('',(9.16515138991168,16.,1.));
#14760=CARTESIAN_POINT('',(7.66515138991168,14.1,4.2));
#14761=CARTESIAN_POINT('',(7.66515138991168,17.9,4.2));
#14762=CARTESIAN_POINT('',(10.6651513899117,14.1,4.2));
#14763=CARTESIAN_POINT('',(10.6651513899117,17.9,4.2));
#14764=CARTESIAN_POINT('',(9.16515138991168,16.,10.));
#14765=CARTESIAN_POINT('',(0.,0.,0.));
#14766=CARTESIAN_POINT('',(0.,0.,0.));
#14767=CARTESIAN_POINT('',(0.,0.,0.));
#14768=CARTESIAN_POINT('',(0.,0.,0.));
#14769=CARTESIAN_POINT('',(0.,0.,0.));
#14770=CARTESIAN_POINT('',(0.,0.,0.));
#14771=UNCERTAINTY_MEASURE_WITH_UNIT(LENGTH_MEASURE(0.001),#14879,
'DISTANCE_ACCURACY_VALUE',
'Maximum model space distance between geometric entities at asserted c
onnectivities');
#14772=UNCERTAINTY_MEASURE_WITH_UNIT(LENGTH_MEASURE(0.001),#14879,
'DISTANCE_ACCURACY_VALUE',
'Maximum model space distance between geometric entities at asserted c
onnectivities');
#14773=UNCERTAINTY_MEASURE_WITH_UNIT(LENGTH_MEASURE(0.001),#14879,
'DISTANCE_ACCURACY_VALUE',
'Maximum model space distance between geometric entities at asserted c
onnectivities');
#14774=UNCERTAINTY_MEASURE_WITH_UNIT(LENGTH_MEASURE(0.001),#14879,
'DISTANCE_ACCURACY_VALUE',
'Maximum model space distance between geometric entities at asserted c
onnectivities');
#14775=UNCERTAINTY_MEASURE_WITH_UNIT(LENGTH_MEASURE(0.001),#14879,
'DISTANCE_ACCURACY_VALUE',
'Maximum model space distance between geometric entities at asserted c
onnectivities');
#14776=UNCERTAINTY_MEASURE_WITH_UNIT(LENGTH_MEASURE(0.001),#14879,
'DISTANCE_ACCURACY_VALUE',
'Maximum model space distance between geometric entities at asserted c
onnectivities');
#14777=UNCERTAINTY_MEASURE_WITH_UNIT(LENGTH_MEASURE(0.001),#14879,
'DISTANCE_ACCURACY_VALUE',
'Maximum model space distance between geometric entities at asserted c
onnectivities');
#14778=UNCERTAINTY_MEASURE_WITH_UNIT(LENGTH_MEASURE(0.001),#14879,
'DISTANCE_ACCURACY_VALUE',
'Maximum model space distance between geometric entities at asserted c
onnectivities');
#14779=UNCERTAINTY_MEASURE_WITH_UNIT(LENGTH_MEASURE(0.001),#14879,
'DISTANCE_ACCURACY_VALUE',
'Maximum model space distance between geometric entities at asserted c
onnectivities');
#14780=UNCERTAINTY_MEASURE_WITH_UNIT(LENGTH_MEASURE(0.001),#14879,
'DISTANCE_ACCURACY_VALUE',
'Maximum model space distance between geometric entities at asserted c
onnectivities');
#14781=UNCERTAINTY_MEASURE_WITH_UNIT(LENGTH_MEASURE(0.001),#14879,
'DISTANCE_ACCURACY_VALUE',
'Maximum model space distance between geometric entities at asserted c
onnectivities');
#14782=UNCERTAINTY_MEASURE_WITH_UNIT(LENGTH_MEASURE(0.001),#14879,
'DISTANCE_ACCURACY_VALUE',
'Maximum model space distance between geometric entities at asserted c
onnectivities');
#14783=UNCERTAINTY_MEASURE_WITH_UNIT(LENGTH_MEASURE(0.001),#14879,
'DISTANCE_ACCURACY_VALUE',
'Maximum model space distance between geometric entities at asserted c
onnectivities');
#14784=UNCERTAINTY_MEASURE_WITH_UNIT(LENGTH_MEASURE(0.001),#14879,
'DISTANCE_ACCURACY_VALUE',
'Maximum model space distance between geometric entities at asserted c
onnectivities');
#14785=UNCERTAINTY_MEASURE_WITH_UNIT(LENGTH_MEASURE(0.001),#14879,
'DISTANCE_ACCURACY_VALUE',
'Maximum model space distance between geometric entities at asserted c
onnectivities');
#14786=UNCERTAINTY_MEASURE_WITH_UNIT(LENGTH_MEASURE(0.001),#14879,
'DISTANCE_ACCURACY_VALUE',
'Maximum model space distance between geometric entities at asserted c
onnectivities');
#14787=UNCERTAINTY_MEASURE_WITH_UNIT(LENGTH_MEASURE(0.001),#14879,
'DISTANCE_ACCURACY_VALUE',
'Maximum model space distance between geometric entities at asserted c
onnectivities');
#14788=UNCERTAINTY_MEASURE_WITH_UNIT(LENGTH_MEASURE(0.001),#14879,
'DISTANCE_ACCURACY_VALUE',
'Maximum model space distance between geometric entities at asserted c
onnectivities');
#14789=UNCERTAINTY_MEASURE_WITH_UNIT(LENGTH_MEASURE(0.001),#14879,
'DISTANCE_ACCURACY_VALUE',
'Maximum model space distance between geometric entities at asserted c
onnectivities');
#14790=UNCERTAINTY_MEASURE_WITH_UNIT(LENGTH_MEASURE(0.001),#14879,
'DISTANCE_ACCURACY_VALUE',
'Maximum model space distance between geometric entities at asserted c
onnectivities');
#14791=UNCERTAINTY_MEASURE_WITH_UNIT(LENGTH_MEASURE(0.001),#14879,
'DISTANCE_ACCURACY_VALUE',
'Maximum model space distance between geometric entities at asserted c
onnectivities');
#14792=UNCERTAINTY_MEASURE_WITH_UNIT(LENGTH_MEASURE(0.001),#14879,
'DISTANCE_ACCURACY_VALUE',
'Maximum model space distance between geometric entities at asserted c
onnectivities');
#14793=UNCERTAINTY_MEASURE_WITH_UNIT(LENGTH_MEASURE(0.001),#14879,
'DISTANCE_ACCURACY_VALUE',
'Maximum model space distance between geometric entities at asserted c
onnectivities');
#14794=UNCERTAINTY_MEASURE_WITH_UNIT(LENGTH_MEASURE(0.001),#14879,
'DISTANCE_ACCURACY_VALUE',
'Maximum model space distance between geometric entities at asserted c
onnectivities');
#14795=UNCERTAINTY_MEASURE_WITH_UNIT(LENGTH_MEASURE(0.001),#14879,
'DISTANCE_ACCURACY_VALUE',
'Maximum model space distance between geometric entities at asserted c
onnectivities');
#14796=UNCERTAINTY_MEASURE_WITH_UNIT(LENGTH_MEASURE(0.001),#14879,
'DISTANCE_ACCURACY_VALUE',
'Maximum model space distance between geometric entities at asserted c
onnectivities');
#14797=UNCERTAINTY_MEASURE_WITH_UNIT(LENGTH_MEASURE(0.001),#14879,
'DISTANCE_ACCURACY_VALUE',
'Maximum model space distance between geometric entities at asserted c
onnectivities');
#14798=UNCERTAINTY_MEASURE_WITH_UNIT(LENGTH_MEASURE(0.001),#14879,
'DISTANCE_ACCURACY_VALUE',
'Maximum model space distance between geometric entities at asserted c
onnectivities');
#14799=UNCERTAINTY_MEASURE_WITH_UNIT(LENGTH_MEASURE(0.001),#14879,
'DISTANCE_ACCURACY_VALUE',
'Maximum model space distance between geometric entities at asserted c
onnectivities');
#14800=UNCERTAINTY_MEASURE_WITH_UNIT(LENGTH_MEASURE(0.001),#14879,
'DISTANCE_ACCURACY_VALUE',
'Maximum model space distance between geometric entities at asserted c
onnectivities');
#14801=UNCERTAINTY_MEASURE_WITH_UNIT(LENGTH_MEASURE(0.001),#14879,
'DISTANCE_ACCURACY_VALUE',
'Maximum model space distance between geometric entities at asserted c
onnectivities');
#14802=UNCERTAINTY_MEASURE_WITH_UNIT(LENGTH_MEASURE(0.001),#14879,
'DISTANCE_ACCURACY_VALUE',
'Maximum model space distance between geometric entities at asserted c
onnectivities');
#14803=UNCERTAINTY_MEASURE_WITH_UNIT(LENGTH_MEASURE(0.001),#14879,
'DISTANCE_ACCURACY_VALUE',
'Maximum model space distance between geometric entities at asserted c
onnectivities');
#14804=UNCERTAINTY_MEASURE_WITH_UNIT(LENGTH_MEASURE(0.001),#14879,
'DISTANCE_ACCURACY_VALUE',
'Maximum model space distance between geometric entities at asserted c
onnectivities');
#14805=UNCERTAINTY_MEASURE_WITH_UNIT(LENGTH_MEASURE(0.001),#14879,
'DISTANCE_ACCURACY_VALUE',
'Maximum model space distance between geometric entities at asserted c
onnectivities');
#14806=UNCERTAINTY_MEASURE_WITH_UNIT(LENGTH_MEASURE(0.001),#14879,
'DISTANCE_ACCURACY_VALUE',
'Maximum model space distance between geometric entities at asserted c
onnectivities');
#14807=UNCERTAINTY_MEASURE_WITH_UNIT(LENGTH_MEASURE(0.001),#14879,
'DISTANCE_ACCURACY_VALUE',
'Maximum model space distance between geometric entities at asserted c
onnectivities');
#14808=UNCERTAINTY_MEASURE_WITH_UNIT(LENGTH_MEASURE(0.001),#14879,
'DISTANCE_ACCURACY_VALUE',
'Maximum model space distance between geometric entities at asserted c
onnectivities');
#14809=UNCERTAINTY_MEASURE_WITH_UNIT(LENGTH_MEASURE(0.001),#14879,
'DISTANCE_ACCURACY_VALUE',
'Maximum model space distance between geometric entities at asserted c
onnectivities');
#14810=UNCERTAINTY_MEASURE_WITH_UNIT(LENGTH_MEASURE(0.001),#14879,
'DISTANCE_ACCURACY_VALUE',
'Maximum model space distance between geometric entities at asserted c
onnectivities');
#14811=UNCERTAINTY_MEASURE_WITH_UNIT(LENGTH_MEASURE(0.001),#14879,
'DISTANCE_ACCURACY_VALUE',
'Maximum model space distance between geometric entities at asserted c
onnectivities');
#14812=UNCERTAINTY_MEASURE_WITH_UNIT(LENGTH_MEASURE(0.001),#14879,
'DISTANCE_ACCURACY_VALUE',
'Maximum model space distance between geometric entities at asserted c
onnectivities');
#14813=UNCERTAINTY_MEASURE_WITH_UNIT(LENGTH_MEASURE(0.001),#14879,
'DISTANCE_ACCURACY_VALUE',
'Maximum model space distance between geometric entities at asserted c
onnectivities');
#14814=UNCERTAINTY_MEASURE_WITH_UNIT(LENGTH_MEASURE(0.001),#14879,
'DISTANCE_ACCURACY_VALUE',
'Maximum model space distance between geometric entities at asserted c
onnectivities');
#14815=UNCERTAINTY_MEASURE_WITH_UNIT(LENGTH_MEASURE(0.001),#14879,
'DISTANCE_ACCURACY_VALUE',
'Maximum model space distance between geometric entities at asserted c
onnectivities');
#14816=UNCERTAINTY_MEASURE_WITH_UNIT(LENGTH_MEASURE(0.001),#14879,
'DISTANCE_ACCURACY_VALUE',
'Maximum model space distance between geometric entities at asserted c
onnectivities');
#14817=UNCERTAINTY_MEASURE_WITH_UNIT(LENGTH_MEASURE(0.001),#14879,
'DISTANCE_ACCURACY_VALUE',
'Maximum model space distance between geometric entities at asserted c
onnectivities');
#14818=UNCERTAINTY_MEASURE_WITH_UNIT(LENGTH_MEASURE(0.001),#14879,
'DISTANCE_ACCURACY_VALUE',
'Maximum model space distance between geometric entities at asserted c
onnectivities');
#14819=UNCERTAINTY_MEASURE_WITH_UNIT(LENGTH_MEASURE(0.001),#14879,
'DISTANCE_ACCURACY_VALUE',
'Maximum model space distance between geometric entities at asserted c
onnectivities');
#14820=UNCERTAINTY_MEASURE_WITH_UNIT(LENGTH_MEASURE(0.001),#14879,
'DISTANCE_ACCURACY_VALUE',
'Maximum model space distance between geometric entities at asserted c
onnectivities');
#14821=UNCERTAINTY_MEASURE_WITH_UNIT(LENGTH_MEASURE(0.001),#14879,
'DISTANCE_ACCURACY_VALUE',
'Maximum model space distance between geometric entities at asserted c
onnectivities');
#14822=UNCERTAINTY_MEASURE_WITH_UNIT(LENGTH_MEASURE(0.001),#14879,
'DISTANCE_ACCURACY_VALUE',
'Maximum model space distance between geometric entities at asserted c
onnectivities');
#14823=UNCERTAINTY_MEASURE_WITH_UNIT(LENGTH_MEASURE(0.001),#14879,
'DISTANCE_ACCURACY_VALUE',
'Maximum model space distance between geometric entities at asserted c
onnectivities');
#14824=UNCERTAINTY_MEASURE_WITH_UNIT(LENGTH_MEASURE(0.001),#14879,
'DISTANCE_ACCURACY_VALUE',
'Maximum model space distance between geometric entities at asserted c
onnectivities');
#14825=(
GEOMETRIC_REPRESENTATION_CONTEXT(3)
GLOBAL_UNCERTAINTY_ASSIGNED_CONTEXT((#14771))
GLOBAL_UNIT_ASSIGNED_CONTEXT((#14879,#14881,#14882))
REPRESENTATION_CONTEXT('','3D')
);
#14826=(
GEOMETRIC_REPRESENTATION_CONTEXT(3)
GLOBAL_UNCERTAINTY_ASSIGNED_CONTEXT((#14772))
GLOBAL_UNIT_ASSIGNED_CONTEXT((#14879,#14881,#14882))
REPRESENTATION_CONTEXT('','3D')
);
#14827=(
GEOMETRIC_REPRESENTATION_CONTEXT(3)
GLOBAL_UNCERTAINTY_ASSIGNED_CONTEXT((#14773))
GLOBAL_UNIT_ASSIGNED_CONTEXT((#14879,#14881,#14882))
REPRESENTATION_CONTEXT('','3D')
);
#14828=(
GEOMETRIC_REPRESENTATION_CONTEXT(3)
GLOBAL_UNCERTAINTY_ASSIGNED_CONTEXT((#14774))
GLOBAL_UNIT_ASSIGNED_CONTEXT((#14879,#14881,#14882))
REPRESENTATION_CONTEXT('','3D')
);
#14829=(
GEOMETRIC_REPRESENTATION_CONTEXT(3)
GLOBAL_UNCERTAINTY_ASSIGNED_CONTEXT((#14775))
GLOBAL_UNIT_ASSIGNED_CONTEXT((#14879,#14881,#14882))
REPRESENTATION_CONTEXT('','3D')
);
#14830=(
GEOMETRIC_REPRESENTATION_CONTEXT(3)
GLOBAL_UNCERTAINTY_ASSIGNED_CONTEXT((#14776))
GLOBAL_UNIT_ASSIGNED_CONTEXT((#14879,#14881,#14882))
REPRESENTATION_CONTEXT('','3D')
);
#14831=(
GEOMETRIC_REPRESENTATION_CONTEXT(3)
GLOBAL_UNCERTAINTY_ASSIGNED_CONTEXT((#14777))
GLOBAL_UNIT_ASSIGNED_CONTEXT((#14879,#14881,#14882))
REPRESENTATION_CONTEXT('','3D')
);
#14832=(
GEOMETRIC_REPRESENTATION_CONTEXT(3)
GLOBAL_UNCERTAINTY_ASSIGNED_CONTEXT((#14778))
GLOBAL_UNIT_ASSIGNED_CONTEXT((#14879,#14881,#14882))
REPRESENTATION_CONTEXT('','3D')
);
#14833=(
GEOMETRIC_REPRESENTATION_CONTEXT(3)
GLOBAL_UNCERTAINTY_ASSIGNED_CONTEXT((#14779))
GLOBAL_UNIT_ASSIGNED_CONTEXT((#14879,#14881,#14882))
REPRESENTATION_CONTEXT('','3D')
);
#14834=(
GEOMETRIC_REPRESENTATION_CONTEXT(3)
GLOBAL_UNCERTAINTY_ASSIGNED_CONTEXT((#14780))
GLOBAL_UNIT_ASSIGNED_CONTEXT((#14879,#14881,#14882))
REPRESENTATION_CONTEXT('','3D')
);
#14835=(
GEOMETRIC_REPRESENTATION_CONTEXT(3)
GLOBAL_UNCERTAINTY_ASSIGNED_CONTEXT((#14781))
GLOBAL_UNIT_ASSIGNED_CONTEXT((#14879,#14881,#14882))
REPRESENTATION_CONTEXT('','3D')
);
#14836=(
GEOMETRIC_REPRESENTATION_CONTEXT(3)
GLOBAL_UNCERTAINTY_ASSIGNED_CONTEXT((#14782))
GLOBAL_UNIT_ASSIGNED_CONTEXT((#14879,#14881,#14882))
REPRESENTATION_CONTEXT('','3D')
);
#14837=(
GEOMETRIC_REPRESENTATION_CONTEXT(3)
GLOBAL_UNCERTAINTY_ASSIGNED_CONTEXT((#14783))
GLOBAL_UNIT_ASSIGNED_CONTEXT((#14879,#14881,#14882))
REPRESENTATION_CONTEXT('','3D')
);
#14838=(
GEOMETRIC_REPRESENTATION_CONTEXT(3)
GLOBAL_UNCERTAINTY_ASSIGNED_CONTEXT((#14784))
GLOBAL_UNIT_ASSIGNED_CONTEXT((#14879,#14881,#14882))
REPRESENTATION_CONTEXT('','3D')
);
#14839=(
GEOMETRIC_REPRESENTATION_CONTEXT(3)
GLOBAL_UNCERTAINTY_ASSIGNED_CONTEXT((#14785))
GLOBAL_UNIT_ASSIGNED_CONTEXT((#14879,#14881,#14882))
REPRESENTATION_CONTEXT('','3D')
);
#14840=(
GEOMETRIC_REPRESENTATION_CONTEXT(3)
GLOBAL_UNCERTAINTY_ASSIGNED_CONTEXT((#14786))
GLOBAL_UNIT_ASSIGNED_CONTEXT((#14879,#14881,#14882))
REPRESENTATION_CONTEXT('','3D')
);
#14841=(
GEOMETRIC_REPRESENTATION_CONTEXT(3)
GLOBAL_UNCERTAINTY_ASSIGNED_CONTEXT((#14787))
GLOBAL_UNIT_ASSIGNED_CONTEXT((#14879,#14881,#14882))
REPRESENTATION_CONTEXT('','3D')
);
#14842=(
GEOMETRIC_REPRESENTATION_CONTEXT(3)
GLOBAL_UNCERTAINTY_ASSIGNED_CONTEXT((#14788))
GLOBAL_UNIT_ASSIGNED_CONTEXT((#14879,#14881,#14882))
REPRESENTATION_CONTEXT('','3D')
);
#14843=(
GEOMETRIC_REPRESENTATION_CONTEXT(3)
GLOBAL_UNCERTAINTY_ASSIGNED_CONTEXT((#14789))
GLOBAL_UNIT_ASSIGNED_CONTEXT((#14879,#14881,#14882))
REPRESENTATION_CONTEXT('','3D')
);
#14844=(
GEOMETRIC_REPRESENTATION_CONTEXT(3)
GLOBAL_UNCERTAINTY_ASSIGNED_CONTEXT((#14790))
GLOBAL_UNIT_ASSIGNED_CONTEXT((#14879,#14881,#14882))
REPRESENTATION_CONTEXT('','3D')
);
#14845=(
GEOMETRIC_REPRESENTATION_CONTEXT(3)
GLOBAL_UNCERTAINTY_ASSIGNED_CONTEXT((#14791))
GLOBAL_UNIT_ASSIGNED_CONTEXT((#14879,#14881,#14882))
REPRESENTATION_CONTEXT('','3D')
);
#14846=(
GEOMETRIC_REPRESENTATION_CONTEXT(3)
GLOBAL_UNCERTAINTY_ASSIGNED_CONTEXT((#14792))
GLOBAL_UNIT_ASSIGNED_CONTEXT((#14879,#14881,#14882))
REPRESENTATION_CONTEXT('','3D')
);
#14847=(
GEOMETRIC_REPRESENTATION_CONTEXT(3)
GLOBAL_UNCERTAINTY_ASSIGNED_CONTEXT((#14793))
GLOBAL_UNIT_ASSIGNED_CONTEXT((#14879,#14881,#14882))
REPRESENTATION_CONTEXT('','3D')
);
#14848=(
GEOMETRIC_REPRESENTATION_CONTEXT(3)
GLOBAL_UNCERTAINTY_ASSIGNED_CONTEXT((#14794))
GLOBAL_UNIT_ASSIGNED_CONTEXT((#14879,#14881,#14882))
REPRESENTATION_CONTEXT('','3D')
);
#14849=(
GEOMETRIC_REPRESENTATION_CONTEXT(3)
GLOBAL_UNCERTAINTY_ASSIGNED_CONTEXT((#14795))
GLOBAL_UNIT_ASSIGNED_CONTEXT((#14879,#14881,#14882))
REPRESENTATION_CONTEXT('','3D')
);
#14850=(
GEOMETRIC_REPRESENTATION_CONTEXT(3)
GLOBAL_UNCERTAINTY_ASSIGNED_CONTEXT((#14796))
GLOBAL_UNIT_ASSIGNED_CONTEXT((#14879,#14881,#14882))
REPRESENTATION_CONTEXT('','3D')
);
#14851=(
GEOMETRIC_REPRESENTATION_CONTEXT(3)
GLOBAL_UNCERTAINTY_ASSIGNED_CONTEXT((#14797))
GLOBAL_UNIT_ASSIGNED_CONTEXT((#14879,#14881,#14882))
REPRESENTATION_CONTEXT('','3D')
);
#14852=(
GEOMETRIC_REPRESENTATION_CONTEXT(3)
GLOBAL_UNCERTAINTY_ASSIGNED_CONTEXT((#14798))
GLOBAL_UNIT_ASSIGNED_CONTEXT((#14879,#14881,#14882))
REPRESENTATION_CONTEXT('','3D')
);
#14853=(
GEOMETRIC_REPRESENTATION_CONTEXT(3)
GLOBAL_UNCERTAINTY_ASSIGNED_CONTEXT((#14799))
GLOBAL_UNIT_ASSIGNED_CONTEXT((#14879,#14881,#14882))
REPRESENTATION_CONTEXT('','3D')
);
#14854=(
GEOMETRIC_REPRESENTATION_CONTEXT(3)
GLOBAL_UNCERTAINTY_ASSIGNED_CONTEXT((#14800))
GLOBAL_UNIT_ASSIGNED_CONTEXT((#14879,#14881,#14882))
REPRESENTATION_CONTEXT('','3D')
);
#14855=(
GEOMETRIC_REPRESENTATION_CONTEXT(3)
GLOBAL_UNCERTAINTY_ASSIGNED_CONTEXT((#14801))
GLOBAL_UNIT_ASSIGNED_CONTEXT((#14879,#14881,#14882))
REPRESENTATION_CONTEXT('','3D')
);
#14856=(
GEOMETRIC_REPRESENTATION_CONTEXT(3)
GLOBAL_UNCERTAINTY_ASSIGNED_CONTEXT((#14802))
GLOBAL_UNIT_ASSIGNED_CONTEXT((#14879,#14881,#14882))
REPRESENTATION_CONTEXT('','3D')
);
#14857=(
GEOMETRIC_REPRESENTATION_CONTEXT(3)
GLOBAL_UNCERTAINTY_ASSIGNED_CONTEXT((#14803))
GLOBAL_UNIT_ASSIGNED_CONTEXT((#14879,#14881,#14882))
REPRESENTATION_CONTEXT('','3D')
);
#14858=(
GEOMETRIC_REPRESENTATION_CONTEXT(3)
GLOBAL_UNCERTAINTY_ASSIGNED_CONTEXT((#14804))
GLOBAL_UNIT_ASSIGNED_CONTEXT((#14879,#14881,#14882))
REPRESENTATION_CONTEXT('','3D')
);
#14859=(
GEOMETRIC_REPRESENTATION_CONTEXT(3)
GLOBAL_UNCERTAINTY_ASSIGNED_CONTEXT((#14805))
GLOBAL_UNIT_ASSIGNED_CONTEXT((#14879,#14881,#14882))
REPRESENTATION_CONTEXT('','3D')
);
#14860=(
GEOMETRIC_REPRESENTATION_CONTEXT(3)
GLOBAL_UNCERTAINTY_ASSIGNED_CONTEXT((#14806))
GLOBAL_UNIT_ASSIGNED_CONTEXT((#14879,#14881,#14882))
REPRESENTATION_CONTEXT('','3D')
);
#14861=(
GEOMETRIC_REPRESENTATION_CONTEXT(3)
GLOBAL_UNCERTAINTY_ASSIGNED_CONTEXT((#14807))
GLOBAL_UNIT_ASSIGNED_CONTEXT((#14879,#14881,#14882))
REPRESENTATION_CONTEXT('','3D')
);
#14862=(
GEOMETRIC_REPRESENTATION_CONTEXT(3)
GLOBAL_UNCERTAINTY_ASSIGNED_CONTEXT((#14808))
GLOBAL_UNIT_ASSIGNED_CONTEXT((#14879,#14881,#14882))
REPRESENTATION_CONTEXT('','3D')
);
#14863=(
GEOMETRIC_REPRESENTATION_CONTEXT(3)
GLOBAL_UNCERTAINTY_ASSIGNED_CONTEXT((#14809))
GLOBAL_UNIT_ASSIGNED_CONTEXT((#14879,#14881,#14882))
REPRESENTATION_CONTEXT('','3D')
);
#14864=(
GEOMETRIC_REPRESENTATION_CONTEXT(3)
GLOBAL_UNCERTAINTY_ASSIGNED_CONTEXT((#14810))
GLOBAL_UNIT_ASSIGNED_CONTEXT((#14879,#14881,#14882))
REPRESENTATION_CONTEXT('','3D')
);
#14865=(
GEOMETRIC_REPRESENTATION_CONTEXT(3)
GLOBAL_UNCERTAINTY_ASSIGNED_CONTEXT((#14811))
GLOBAL_UNIT_ASSIGNED_CONTEXT((#14879,#14881,#14882))
REPRESENTATION_CONTEXT('','3D')
);
#14866=(
GEOMETRIC_REPRESENTATION_CONTEXT(3)
GLOBAL_UNCERTAINTY_ASSIGNED_CONTEXT((#14812))
GLOBAL_UNIT_ASSIGNED_CONTEXT((#14879,#14881,#14882))
REPRESENTATION_CONTEXT('','3D')
);
#14867=(
GEOMETRIC_REPRESENTATION_CONTEXT(3)
GLOBAL_UNCERTAINTY_ASSIGNED_CONTEXT((#14813))
GLOBAL_UNIT_ASSIGNED_CONTEXT((#14879,#14881,#14882))
REPRESENTATION_CONTEXT('','3D')
);
#14868=(
GEOMETRIC_REPRESENTATION_CONTEXT(3)
GLOBAL_UNCERTAINTY_ASSIGNED_CONTEXT((#14814))
GLOBAL_UNIT_ASSIGNED_CONTEXT((#14879,#14881,#14882))
REPRESENTATION_CONTEXT('','3D')
);
#14869=(
GEOMETRIC_REPRESENTATION_CONTEXT(3)
GLOBAL_UNCERTAINTY_ASSIGNED_CONTEXT((#14815))
GLOBAL_UNIT_ASSIGNED_CONTEXT((#14879,#14881,#14882))
REPRESENTATION_CONTEXT('','3D')
);
#14870=(
GEOMETRIC_REPRESENTATION_CONTEXT(3)
GLOBAL_UNCERTAINTY_ASSIGNED_CONTEXT((#14816))
GLOBAL_UNIT_ASSIGNED_CONTEXT((#14879,#14881,#14882))
REPRESENTATION_CONTEXT('','3D')
);
#14871=(
GEOMETRIC_REPRESENTATION_CONTEXT(3)
GLOBAL_UNCERTAINTY_ASSIGNED_CONTEXT((#14817))
GLOBAL_UNIT_ASSIGNED_CONTEXT((#14879,#14881,#14882))
REPRESENTATION_CONTEXT('','3D')
);
#14872=(
GEOMETRIC_REPRESENTATION_CONTEXT(3)
GLOBAL_UNCERTAINTY_ASSIGNED_CONTEXT((#14818))
GLOBAL_UNIT_ASSIGNED_CONTEXT((#14879,#14881,#14882))
REPRESENTATION_CONTEXT('','3D')
);
#14873=(
GEOMETRIC_REPRESENTATION_CONTEXT(3)
GLOBAL_UNCERTAINTY_ASSIGNED_CONTEXT((#14819))
GLOBAL_UNIT_ASSIGNED_CONTEXT((#14879,#14881,#14882))
REPRESENTATION_CONTEXT('','3D')
);
#14874=(
GEOMETRIC_REPRESENTATION_CONTEXT(3)
GLOBAL_UNCERTAINTY_ASSIGNED_CONTEXT((#14820))
GLOBAL_UNIT_ASSIGNED_CONTEXT((#14879,#14881,#14882))
REPRESENTATION_CONTEXT('','3D')
);
#14875=(
GEOMETRIC_REPRESENTATION_CONTEXT(3)
GLOBAL_UNCERTAINTY_ASSIGNED_CONTEXT((#14821))
GLOBAL_UNIT_ASSIGNED_CONTEXT((#14879,#14881,#14882))
REPRESENTATION_CONTEXT('','3D')
);
#14876=(
GEOMETRIC_REPRESENTATION_CONTEXT(3)
GLOBAL_UNCERTAINTY_ASSIGNED_CONTEXT((#14822))
GLOBAL_UNIT_ASSIGNED_CONTEXT((#14879,#14881,#14882))
REPRESENTATION_CONTEXT('','3D')
);
#14877=(
GEOMETRIC_REPRESENTATION_CONTEXT(3)
GLOBAL_UNCERTAINTY_ASSIGNED_CONTEXT((#14823))
GLOBAL_UNIT_ASSIGNED_CONTEXT((#14879,#14881,#14882))
REPRESENTATION_CONTEXT('','3D')
);
#14878=(
GEOMETRIC_REPRESENTATION_CONTEXT(3)
GLOBAL_UNCERTAINTY_ASSIGNED_CONTEXT((#14824))
GLOBAL_UNIT_ASSIGNED_CONTEXT((#14879,#14881,#14882))
REPRESENTATION_CONTEXT('','3D')
);
#14879=(
LENGTH_UNIT()
NAMED_UNIT(*)
SI_UNIT(.CENTI.,.METRE.)
);
#14880=(
LENGTH_UNIT()
NAMED_UNIT(*)
SI_UNIT($,.METRE.)
);
#14881=(
NAMED_UNIT(*)
PLANE_ANGLE_UNIT()
SI_UNIT($,.RADIAN.)
);
#14882=(
NAMED_UNIT(*)
SI_UNIT($,.STERADIAN.)
SOLID_ANGLE_UNIT()
);
#14883=SHAPE_DEFINITION_REPRESENTATION(#14936,#15068);
#14884=SHAPE_DEFINITION_REPRESENTATION(#14937,#15069);
#14885=SHAPE_DEFINITION_REPRESENTATION(#14938,#15070);
#14886=SHAPE_DEFINITION_REPRESENTATION(#14939,#15071);
#14887=SHAPE_DEFINITION_REPRESENTATION(#14940,#15072);
#14888=SHAPE_DEFINITION_REPRESENTATION(#14941,#15073);
#14889=SHAPE_DEFINITION_REPRESENTATION(#14942,#15074);
#14890=SHAPE_DEFINITION_REPRESENTATION(#14943,#15075);
#14891=SHAPE_DEFINITION_REPRESENTATION(#14944,#15076);
#14892=SHAPE_DEFINITION_REPRESENTATION(#14945,#15077);
#14893=SHAPE_DEFINITION_REPRESENTATION(#14946,#15078);
#14894=SHAPE_DEFINITION_REPRESENTATION(#14947,#15079);
#14895=SHAPE_DEFINITION_REPRESENTATION(#14948,#15080);
#14896=SHAPE_DEFINITION_REPRESENTATION(#14949,#15081);
#14897=SHAPE_DEFINITION_REPRESENTATION(#14950,#15082);
#14898=SHAPE_DEFINITION_REPRESENTATION(#14951,#15083);
#14899=SHAPE_DEFINITION_REPRESENTATION(#14957,#15084);
#14900=SHAPE_DEFINITION_REPRESENTATION(#14958,#15085);
#14901=SHAPE_DEFINITION_REPRESENTATION(#14959,#15086);
#14902=SHAPE_DEFINITION_REPRESENTATION(#14960,#15087);
#14903=SHAPE_DEFINITION_REPRESENTATION(#14961,#15088);
#14904=SHAPE_DEFINITION_REPRESENTATION(#14962,#15089);
#14905=SHAPE_DEFINITION_REPRESENTATION(#14963,#15090);
#14906=SHAPE_DEFINITION_REPRESENTATION(#14964,#15091);
#14907=SHAPE_DEFINITION_REPRESENTATION(#14965,#15092);
#14908=SHAPE_DEFINITION_REPRESENTATION(#14966,#15093);
#14909=SHAPE_DEFINITION_REPRESENTATION(#14967,#15094);
#14910=SHAPE_DEFINITION_REPRESENTATION(#14968,#15095);
#14911=SHAPE_DEFINITION_REPRESENTATION(#14969,#15096);
#14912=SHAPE_DEFINITION_REPRESENTATION(#14970,#15097);
#14913=SHAPE_DEFINITION_REPRESENTATION(#14971,#15098);
#14914=SHAPE_DEFINITION_REPRESENTATION(#14972,#15099);
#14915=SHAPE_DEFINITION_REPRESENTATION(#14973,#15100);
#14916=SHAPE_DEFINITION_REPRESENTATION(#14974,#15101);
#14917=SHAPE_DEFINITION_REPRESENTATION(#14975,#15102);
#14918=SHAPE_DEFINITION_REPRESENTATION(#14976,#15103);
#14919=SHAPE_DEFINITION_REPRESENTATION(#14977,#15104);
#14920=SHAPE_DEFINITION_REPRESENTATION(#14979,#15105);
#14921=SHAPE_DEFINITION_REPRESENTATION(#14980,#15106);
#14922=SHAPE_DEFINITION_REPRESENTATION(#14981,#15107);
#14923=SHAPE_DEFINITION_REPRESENTATION(#14982,#15108);
#14924=SHAPE_DEFINITION_REPRESENTATION(#14986,#15109);
#14925=SHAPE_DEFINITION_REPRESENTATION(#14987,#15110);
#14926=SHAPE_DEFINITION_REPRESENTATION(#14988,#15111);
#14927=SHAPE_DEFINITION_REPRESENTATION(#14989,#15112);
#14928=SHAPE_DEFINITION_REPRESENTATION(#14990,#15113);
#14929=SHAPE_DEFINITION_REPRESENTATION(#14991,#15114);
#14930=SHAPE_DEFINITION_REPRESENTATION(#14992,#15115);
#14931=SHAPE_DEFINITION_REPRESENTATION(#14993,#15116);
#14932=SHAPE_DEFINITION_REPRESENTATION(#14994,#15117);
#14933=SHAPE_DEFINITION_REPRESENTATION(#14995,#15118);
#14934=SHAPE_DEFINITION_REPRESENTATION(#14999,#15119);
#14935=SHAPE_DEFINITION_REPRESENTATION(#15000,#15120);
#14936=PRODUCT_DEFINITION_SHAPE('',$,#15122);
#14937=PRODUCT_DEFINITION_SHAPE('',$,#15123);
#14938=PRODUCT_DEFINITION_SHAPE('',$,#15124);
#14939=PRODUCT_DEFINITION_SHAPE('',$,#15125);
#14940=PRODUCT_DEFINITION_SHAPE('',$,#15126);
#14941=PRODUCT_DEFINITION_SHAPE('',$,#15127);
#14942=PRODUCT_DEFINITION_SHAPE('',$,#15128);
#14943=PRODUCT_DEFINITION_SHAPE('',$,#15129);
#14944=PRODUCT_DEFINITION_SHAPE('',$,#15130);
#14945=PRODUCT_DEFINITION_SHAPE('',$,#15131);
#14946=PRODUCT_DEFINITION_SHAPE('',$,#15132);
#14947=PRODUCT_DEFINITION_SHAPE('',$,#15133);
#14948=PRODUCT_DEFINITION_SHAPE('',$,#15134);
#14949=PRODUCT_DEFINITION_SHAPE('',$,#15135);
#14950=PRODUCT_DEFINITION_SHAPE('',$,#15136);
#14951=PRODUCT_DEFINITION_SHAPE('',$,#15137);
#14952=PRODUCT_DEFINITION_SHAPE($,$,#254);
#14953=PRODUCT_DEFINITION_SHAPE($,$,#255);
#14954=PRODUCT_DEFINITION_SHAPE($,$,#256);
#14955=PRODUCT_DEFINITION_SHAPE($,$,#257);
#14956=PRODUCT_DEFINITION_SHAPE($,$,#258);
#14957=PRODUCT_DEFINITION_SHAPE('',$,#15138);
#14958=PRODUCT_DEFINITION_SHAPE('',$,#15139);
#14959=PRODUCT_DEFINITION_SHAPE('',$,#15140);
#14960=PRODUCT_DEFINITION_SHAPE('',$,#15141);
#14961=PRODUCT_DEFINITION_SHAPE('',$,#15142);
#14962=PRODUCT_DEFINITION_SHAPE('',$,#15143);
#14963=PRODUCT_DEFINITION_SHAPE('',$,#15144);
#14964=PRODUCT_DEFINITION_SHAPE('',$,#15145);
#14965=PRODUCT_DEFINITION_SHAPE('',$,#15146);
#14966=PRODUCT_DEFINITION_SHAPE('',$,#15147);
#14967=PRODUCT_DEFINITION_SHAPE('',$,#15148);
#14968=PRODUCT_DEFINITION_SHAPE('',$,#15149);
#14969=PRODUCT_DEFINITION_SHAPE('',$,#15150);
#14970=PRODUCT_DEFINITION_SHAPE('',$,#15151);
#14971=PRODUCT_DEFINITION_SHAPE('',$,#15152);
#14972=PRODUCT_DEFINITION_SHAPE('',$,#15153);
#14973=PRODUCT_DEFINITION_SHAPE('',$,#15154);
#14974=PRODUCT_DEFINITION_SHAPE('',$,#15155);
#14975=PRODUCT_DEFINITION_SHAPE('',$,#15156);
#14976=PRODUCT_DEFINITION_SHAPE('',$,#15157);
#14977=PRODUCT_DEFINITION_SHAPE('',$,#15158);
#14978=PRODUCT_DEFINITION_SHAPE($,$,#259);
#14979=PRODUCT_DEFINITION_SHAPE('',$,#15159);
#14980=PRODUCT_DEFINITION_SHAPE('',$,#15160);
#14981=PRODUCT_DEFINITION_SHAPE('',$,#15161);
#14982=PRODUCT_DEFINITION_SHAPE('',$,#15162);
#14983=PRODUCT_DEFINITION_SHAPE($,$,#260);
#14984=PRODUCT_DEFINITION_SHAPE($,$,#261);
#14985=PRODUCT_DEFINITION_SHAPE($,$,#262);
#14986=PRODUCT_DEFINITION_SHAPE('',$,#15163);
#14987=PRODUCT_DEFINITION_SHAPE('',$,#15164);
#14988=PRODUCT_DEFINITION_SHAPE('',$,#15165);
#14989=PRODUCT_DEFINITION_SHAPE('',$,#15166);
#14990=PRODUCT_DEFINITION_SHAPE('',$,#15167);
#14991=PRODUCT_DEFINITION_SHAPE('',$,#15168);
#14992=PRODUCT_DEFINITION_SHAPE('',$,#15169);
#14993=PRODUCT_DEFINITION_SHAPE('',$,#15170);
#14994=PRODUCT_DEFINITION_SHAPE('',$,#15171);
#14995=PRODUCT_DEFINITION_SHAPE('',$,#15172);
#14996=PRODUCT_DEFINITION_SHAPE($,$,#263);
#14997=PRODUCT_DEFINITION_SHAPE($,$,#264);
#14998=PRODUCT_DEFINITION_SHAPE($,$,#265);
#14999=PRODUCT_DEFINITION_SHAPE('',$,#15173);
#15000=PRODUCT_DEFINITION_SHAPE('',$,#15174);
#15001=PRODUCT_DEFINITION_SHAPE($,$,#266);
#15002=PRODUCT_DEFINITION_SHAPE($,$,#267);
#15003=PRODUCT_DEFINITION_SHAPE($,$,#268);
#15004=PRODUCT_DEFINITION_SHAPE($,$,#269);
#15005=PRODUCT_DEFINITION_SHAPE($,$,#270);
#15006=PRODUCT_DEFINITION_SHAPE($,$,#271);
#15007=PRODUCT_DEFINITION_SHAPE($,$,#272);
#15008=PRODUCT_DEFINITION_SHAPE($,$,#273);
#15009=PRODUCT_DEFINITION_SHAPE($,$,#274);
#15010=PRODUCT_DEFINITION_SHAPE($,$,#275);
#15011=PRODUCT_DEFINITION_SHAPE($,$,#276);
#15012=PRODUCT_DEFINITION_SHAPE($,$,#277);
#15013=PRODUCT_DEFINITION_SHAPE($,$,#278);
#15014=PRODUCT_DEFINITION_SHAPE($,$,#279);
#15015=PRODUCT_DEFINITION_SHAPE($,$,#280);
#15016=PRODUCT_DEFINITION_SHAPE($,$,#281);
#15017=PRODUCT_DEFINITION_SHAPE($,$,#282);
#15018=PRODUCT_DEFINITION_SHAPE($,$,#283);
#15019=PRODUCT_DEFINITION_SHAPE($,$,#284);
#15020=PRODUCT_DEFINITION_SHAPE($,$,#285);
#15021=PRODUCT_DEFINITION_SHAPE($,$,#286);
#15022=PRODUCT_DEFINITION_SHAPE($,$,#287);
#15023=PRODUCT_DEFINITION_SHAPE($,$,#288);
#15024=PRODUCT_DEFINITION_SHAPE($,$,#289);
#15025=PRODUCT_DEFINITION_SHAPE($,$,#290);
#15026=PRODUCT_DEFINITION_SHAPE($,$,#291);
#15027=PRODUCT_DEFINITION_SHAPE($,$,#292);
#15028=PRODUCT_DEFINITION_SHAPE($,$,#293);
#15029=PRODUCT_DEFINITION_SHAPE($,$,#294);
#15030=PRODUCT_DEFINITION_SHAPE($,$,#295);
#15031=PRODUCT_DEFINITION_SHAPE($,$,#296);
#15032=PRODUCT_DEFINITION_SHAPE($,$,#297);
#15033=PRODUCT_DEFINITION_SHAPE($,$,#298);
#15034=PRODUCT_DEFINITION_SHAPE($,$,#299);
#15035=PRODUCT_DEFINITION_SHAPE($,$,#300);
#15036=PRODUCT_DEFINITION_SHAPE($,$,#301);
#15037=PRODUCT_DEFINITION_SHAPE($,$,#302);
#15038=PRODUCT_DEFINITION_SHAPE($,$,#303);
#15039=PRODUCT_DEFINITION_SHAPE($,$,#304);
#15040=PRODUCT_DEFINITION_SHAPE($,$,#305);
#15041=PRODUCT_DEFINITION_SHAPE($,$,#306);
#15042=PRODUCT_DEFINITION_SHAPE($,$,#307);
#15043=PRODUCT_DEFINITION_SHAPE($,$,#308);
#15044=PRODUCT_DEFINITION_SHAPE($,$,#309);
#15045=PRODUCT_DEFINITION_SHAPE($,$,#310);
#15046=PRODUCT_DEFINITION_SHAPE($,$,#311);
#15047=PRODUCT_DEFINITION_SHAPE($,$,#312);
#15048=PRODUCT_DEFINITION_SHAPE($,$,#313);
#15049=PRODUCT_DEFINITION_SHAPE($,$,#314);
#15050=PRODUCT_DEFINITION_SHAPE($,$,#315);
#15051=PRODUCT_DEFINITION_SHAPE($,$,#316);
#15052=PRODUCT_DEFINITION_SHAPE($,$,#317);
#15053=PRODUCT_DEFINITION_SHAPE($,$,#318);
#15054=PRODUCT_DEFINITION_SHAPE($,$,#319);
#15055=PRODUCT_DEFINITION_SHAPE($,$,#320);
#15056=PRODUCT_DEFINITION_SHAPE($,$,#321);
#15057=PRODUCT_DEFINITION_SHAPE($,$,#322);
#15058=PRODUCT_DEFINITION_SHAPE($,$,#323);
#15059=PRODUCT_DEFINITION_SHAPE($,$,#324);
#15060=PRODUCT_DEFINITION_SHAPE($,$,#325);
#15061=PRODUCT_DEFINITION_SHAPE($,$,#326);
#15062=PRODUCT_DEFINITION_SHAPE($,$,#327);
#15063=PRODUCT_DEFINITION_SHAPE($,$,#328);
#15064=PRODUCT_DEFINITION_SHAPE($,$,#329);
#15065=PRODUCT_DEFINITION_SHAPE($,$,#330);
#15066=PRODUCT_DEFINITION_SHAPE($,$,#331);
#15067=PRODUCT_DEFINITION_SHAPE($,$,#332);
#15068=SHAPE_REPRESENTATION('',(#8384,#9391,#9392,#9393,#9394,#9395,#9396),
#14825);
#15069=SHAPE_REPRESENTATION('',(#8385,#9330,#9331,#9332,#9333,#9334,#9335,
#9336,#9337,#9338,#9339,#9340,#9341,#9342,#9343,#9344,#9345,#9346,#9347,
#9348,#9349,#9350,#9351,#9352,#9353,#9354,#9355,#9356,#9357,#9358,#9359),
#14826);
#15070=SHAPE_REPRESENTATION('',(#8386),#14827);
#15071=SHAPE_REPRESENTATION('',(#8429),#14828);
#15072=SHAPE_REPRESENTATION('',(#8436),#14829);
#15073=SHAPE_REPRESENTATION('',(#8443),#14830);
#15074=SHAPE_REPRESENTATION('',(#8513),#14831);
#15075=SHAPE_REPRESENTATION('',(#8554),#14832);
#15076=SHAPE_REPRESENTATION('',(#8624),#14833);
#15077=SHAPE_REPRESENTATION('',(#8665),#14834);
#15078=SHAPE_REPRESENTATION('',(#8708,#8837,#8838,#8839,#8840,#8841),#14835);
#15079=SHAPE_REPRESENTATION('',(#8709),#14836);
#15080=SHAPE_REPRESENTATION('',(#8729),#14837);
#15081=SHAPE_REPRESENTATION('',(#8749),#14838);
#15082=SHAPE_REPRESENTATION('',(#8766),#14839);
#15083=SHAPE_REPRESENTATION('',(#8820),#14840);
#15084=SHAPE_REPRESENTATION('',(#8842,#9360,#9361,#9362,#9363,#9364,#9365,
#9366,#9367,#9368,#9369,#9370),#14841);
#15085=SHAPE_REPRESENTATION('',(#8843),#14842);
#15086=SHAPE_REPRESENTATION('',(#8876),#14843);
#15087=SHAPE_REPRESENTATION('',(#8886),#14844);
#15088=SHAPE_REPRESENTATION('',(#8895),#14845);
#15089=SHAPE_REPRESENTATION('',(#8909),#14846);
#15090=SHAPE_REPRESENTATION('',(#8927),#14847);
#15091=SHAPE_REPRESENTATION('',(#8936),#14848);
#15092=SHAPE_REPRESENTATION('',(#8945),#14849);
#15093=SHAPE_REPRESENTATION('',(#8954),#14850);
#15094=SHAPE_REPRESENTATION('',(#8980,#9371,#9372,#9373,#9374,#9375,#9376,
#9377,#9378,#9379),#14851);
#15095=SHAPE_REPRESENTATION('',(#8981),#14852);
#15096=SHAPE_REPRESENTATION('',(#9007),#14853);
#15097=SHAPE_REPRESENTATION('',(#9016),#14854);
#15098=SHAPE_REPRESENTATION('',(#9030),#14855);
#15099=SHAPE_REPRESENTATION('',(#9048),#14856);
#15100=SHAPE_REPRESENTATION('',(#9057),#14857);
#15101=SHAPE_REPRESENTATION('',(#9066),#14858);
#15102=SHAPE_REPRESENTATION('',(#9075),#14859);
#15103=SHAPE_REPRESENTATION('',(#9090,#9109),#14860);
#15104=SHAPE_REPRESENTATION('',(#9091),#14861);
#15105=SHAPE_REPRESENTATION('',(#9110,#9146,#9147,#9148),#14862);
#15106=SHAPE_REPRESENTATION('',(#9111),#14863);
#15107=SHAPE_REPRESENTATION('',(#9128),#14864);
#15108=SHAPE_REPRESENTATION('',(#9137),#14865);
#15109=SHAPE_REPRESENTATION('',(#9149,#9380,#9381,#9382,#9383,#9384,#9385,
#9386,#9387,#9388,#9389,#9390),#14866);
#15110=SHAPE_REPRESENTATION('',(#9150),#14867);
#15111=SHAPE_REPRESENTATION('',(#9172),#14868);
#15112=SHAPE_REPRESENTATION('',(#9190),#14869);
#15113=SHAPE_REPRESENTATION('',(#9199),#14870);
#15114=SHAPE_REPRESENTATION('',(#9208),#14871);
#15115=SHAPE_REPRESENTATION('',(#9217,#9279,#9280,#9281),#14872);
#15116=SHAPE_REPRESENTATION('',(#9218),#14873);
#15117=SHAPE_REPRESENTATION('',(#9257),#14874);
#15118=SHAPE_REPRESENTATION('',(#9268),#14875);
#15119=SHAPE_REPRESENTATION('',(#9282),#14876);
#15120=SHAPE_REPRESENTATION('',(#9306),#14877);
#15121=PRODUCT_DEFINITION_CONTEXT('part definition',#15282,'design');
#15122=PRODUCT_DEFINITION('PAT-084',
'PAT-084',#15175,#15121);
#15123=PRODUCT_DEFINITION('Bearing base and output rail',
'Bearing base and output rail',#15176,#15121);
#15124=PRODUCT_DEFINITION('Base','Base',#15177,#15121);
#15125=PRODUCT_DEFINITION('Foot strip','Foot strip',#15178,#15121);
#15126=PRODUCT_DEFINITION('Foot strip (1)','Foot strip (1)',#15179,#15121);
#15127=PRODUCT_DEFINITION('Lever bearing post','Lever bearing post',#15180,
#15121);
#15128=PRODUCT_DEFINITION('Bearing cap','Bearing cap',#15181,#15121);
#15129=PRODUCT_DEFINITION('Crank bearing post','Crank bearing post',#15182,
#15121);
#15130=PRODUCT_DEFINITION('Bearing cap (1)','Bearing cap (1)',#15183,#15121);
#15131=PRODUCT_DEFINITION('Linear Guide Rail - 15 mm, 220 mm Long',
'Linear Guide Rail - 15 mm, 220 mm Long',#15184,#15121);
#15132=PRODUCT_DEFINITION('Sealed Ball Bearing - 10 x 30 x 9 mm',
'Sealed Ball Bearing - 10 x 30 x 9 mm',#15185,#15121);
#15133=PRODUCT_DEFINITION('Inner ring','Inner ring',#15186,#15121);
#15134=PRODUCT_DEFINITION('Outer ring','Outer ring',#15187,#15121);
#15135=PRODUCT_DEFINITION('Balls','Balls',#15188,#15121);
#15136=PRODUCT_DEFINITION('Cage','Cage',#15189,#15121);
#15137=PRODUCT_DEFINITION('Seals 2RS','Seals 2RS',#15190,#15121);
#15138=PRODUCT_DEFINITION('Driving crank','Driving crank',#15191,#15121);
#15139=PRODUCT_DEFINITION('Input crank and spindle',
'Input crank and spindle',#15192,#15121);
#15140=PRODUCT_DEFINITION('Underside input grip','Underside input grip',
#15193,#15121);
#15141=PRODUCT_DEFINITION('Lower bearing sleeve','Lower bearing sleeve',
#15194,#15121);
#15142=PRODUCT_DEFINITION('Shaft collar','Shaft collar',#15195,#15121);
#15143=PRODUCT_DEFINITION('Crank pin','Crank pin',#15196,#15121);
#15144=PRODUCT_DEFINITION('Crank lower spacer','Crank lower spacer',#15197,
#15121);
#15145=PRODUCT_DEFINITION('Pin upper spacer','Pin upper spacer',#15198,
#15121);
#15146=PRODUCT_DEFINITION('Pin keeper','Pin keeper',#15199,#15121);
#15147=PRODUCT_DEFINITION('Cap Screw - M4x16','Cap Screw - M4x16',#15200,
#15121);
#15148=PRODUCT_DEFINITION('Slotted lever','Slotted lever',#15201,#15121);
#15149=PRODUCT_DEFINITION('Slotted lever and spindle',
'Slotted lever and spindle',#15202,#15121);
#15150=PRODUCT_DEFINITION('Lower bearing sleeve (1)',
'Lower bearing sleeve (1)',#15203,#15121);
#15151=PRODUCT_DEFINITION('Shaft collar (1)','Shaft collar (1)',#15204,#15121);
#15152=PRODUCT_DEFINITION('Lever output pin','Lever output pin',#15205,
#15121);
#15153=PRODUCT_DEFINITION('Lever output lower spacer',
'Lever output lower spacer',#15206,#15121);
#15154=PRODUCT_DEFINITION('Pin upper spacer (1)','Pin upper spacer (1)',#15207,
#15121);
#15155=PRODUCT_DEFINITION('Pin keeper (1)','Pin keeper (1)',#15208,#15121);
#15156=PRODUCT_DEFINITION('M4x4 collar screw','M4x4 collar screw',#15209,
#15121);
#15157=PRODUCT_DEFINITION('Sliding crank block','Sliding crank block',#15210,
#15121);
#15158=PRODUCT_DEFINITION('Captive sliding block',
'Captive sliding block',#15211,#15121);
#15159=PRODUCT_DEFINITION('Output link','Output link',#15212,#15121);
#15160=PRODUCT_DEFINITION('Connecting link','Connecting link',#15213,#15121);
#15161=PRODUCT_DEFINITION('Link bushing','Link bushing',#15214,#15121);
#15162=PRODUCT_DEFINITION('Link bushing (1)','Link bushing (1)',#15215,#15121);
#15163=PRODUCT_DEFINITION('Guided output ram','Guided output ram',#15216,
#15121);
#15164=PRODUCT_DEFINITION('Ram table','Ram table',#15217,#15121);
#15165=PRODUCT_DEFINITION('Ram pin','Ram pin',#15218,#15121);
#15166=PRODUCT_DEFINITION('Ram lower spacer','Ram lower spacer',#15219,
#15121);
#15167=PRODUCT_DEFINITION('Pin upper spacer (2)','Pin upper spacer (2)',#15220,
#15121);
#15168=PRODUCT_DEFINITION('Pin keeper (2)','Pin keeper (2)',#15221,#15121);
#15169=PRODUCT_DEFINITION('Flanged Linear Guide Carriage - 15 mm',
'Flanged Linear Guide Carriage - 15 mm',#15222,#15121);
#15170=PRODUCT_DEFINITION('Block','Block',#15223,#15121);
#15171=PRODUCT_DEFINITION('End cap +','End cap +',#15224,#15121);
#15172=PRODUCT_DEFINITION('End cap','End cap',#15225,#15121);
#15173=PRODUCT_DEFINITION('M5x14 Cap Screw','M5x14 Cap Screw',#15226,#15121);
#15174=PRODUCT_DEFINITION('M4x10 Cap Screw','M4x10 Cap Screw',#15227,#15121);
#15175=PRODUCT_DEFINITION_FORMATION('',$,#15284);
#15176=PRODUCT_DEFINITION_FORMATION('',$,#15285);
#15177=PRODUCT_DEFINITION_FORMATION('',$,#15286);
#15178=PRODUCT_DEFINITION_FORMATION('',$,#15287);
#15179=PRODUCT_DEFINITION_FORMATION('',$,#15288);
#15180=PRODUCT_DEFINITION_FORMATION('',$,#15289);
#15181=PRODUCT_DEFINITION_FORMATION('',$,#15290);
#15182=PRODUCT_DEFINITION_FORMATION('',$,#15291);
#15183=PRODUCT_DEFINITION_FORMATION('',$,#15292);
#15184=PRODUCT_DEFINITION_FORMATION('',$,#15293);
#15185=PRODUCT_DEFINITION_FORMATION('',$,#15294);
#15186=PRODUCT_DEFINITION_FORMATION('',$,#15295);
#15187=PRODUCT_DEFINITION_FORMATION('',$,#15296);
#15188=PRODUCT_DEFINITION_FORMATION('',$,#15297);
#15189=PRODUCT_DEFINITION_FORMATION('',$,#15298);
#15190=PRODUCT_DEFINITION_FORMATION('',$,#15299);
#15191=PRODUCT_DEFINITION_FORMATION('',$,#15300);
#15192=PRODUCT_DEFINITION_FORMATION('',$,#15301);
#15193=PRODUCT_DEFINITION_FORMATION('',$,#15302);
#15194=PRODUCT_DEFINITION_FORMATION('',$,#15303);
#15195=PRODUCT_DEFINITION_FORMATION('',$,#15304);
#15196=PRODUCT_DEFINITION_FORMATION('',$,#15305);
#15197=PRODUCT_DEFINITION_FORMATION('',$,#15306);
#15198=PRODUCT_DEFINITION_FORMATION('',$,#15307);
#15199=PRODUCT_DEFINITION_FORMATION('',$,#15308);
#15200=PRODUCT_DEFINITION_FORMATION('',$,#15309);
#15201=PRODUCT_DEFINITION_FORMATION('',$,#15310);
#15202=PRODUCT_DEFINITION_FORMATION('',$,#15311);
#15203=PRODUCT_DEFINITION_FORMATION('',$,#15312);
#15204=PRODUCT_DEFINITION_FORMATION('',$,#15313);
#15205=PRODUCT_DEFINITION_FORMATION('',$,#15314);
#15206=PRODUCT_DEFINITION_FORMATION('',$,#15315);
#15207=PRODUCT_DEFINITION_FORMATION('',$,#15316);
#15208=PRODUCT_DEFINITION_FORMATION('',$,#15317);
#15209=PRODUCT_DEFINITION_FORMATION('',$,#15318);
#15210=PRODUCT_DEFINITION_FORMATION('',$,#15319);
#15211=PRODUCT_DEFINITION_FORMATION('',$,#15320);
#15212=PRODUCT_DEFINITION_FORMATION('',$,#15321);
#15213=PRODUCT_DEFINITION_FORMATION('',$,#15322);
#15214=PRODUCT_DEFINITION_FORMATION('',$,#15323);
#15215=PRODUCT_DEFINITION_FORMATION('',$,#15324);
#15216=PRODUCT_DEFINITION_FORMATION('',$,#15325);
#15217=PRODUCT_DEFINITION_FORMATION('',$,#15326);
#15218=PRODUCT_DEFINITION_FORMATION('',$,#15327);
#15219=PRODUCT_DEFINITION_FORMATION('',$,#15328);
#15220=PRODUCT_DEFINITION_FORMATION('',$,#15329);
#15221=PRODUCT_DEFINITION_FORMATION('',$,#15330);
#15222=PRODUCT_DEFINITION_FORMATION('',$,#15331);
#15223=PRODUCT_DEFINITION_FORMATION('',$,#15332);
#15224=PRODUCT_DEFINITION_FORMATION('',$,#15333);
#15225=PRODUCT_DEFINITION_FORMATION('',$,#15334);
#15226=PRODUCT_DEFINITION_FORMATION('',$,#15335);
#15227=PRODUCT_DEFINITION_FORMATION('',$,#15336);
#15228=PRODUCT_RELATED_PRODUCT_CATEGORY('PAT-084','PAT-084',(#15284));
#15229=PRODUCT_RELATED_PRODUCT_CATEGORY('Bearing base and output rail',
'Bearing base and output rail',(#15285));
#15230=PRODUCT_RELATED_PRODUCT_CATEGORY('Base','Base',(#15286));
#15231=PRODUCT_RELATED_PRODUCT_CATEGORY('Foot strip','Foot strip',(#15287));
#15232=PRODUCT_RELATED_PRODUCT_CATEGORY('Foot strip (1)',
'Foot strip (1)',(#15288));
#15233=PRODUCT_RELATED_PRODUCT_CATEGORY('Lever bearing post',
'Lever bearing post',(#15289));
#15234=PRODUCT_RELATED_PRODUCT_CATEGORY('Bearing cap','Bearing cap',(#15290));
#15235=PRODUCT_RELATED_PRODUCT_CATEGORY('Crank bearing post',
'Crank bearing post',(#15291));
#15236=PRODUCT_RELATED_PRODUCT_CATEGORY('Bearing cap (1)',
'Bearing cap (1)',(#15292));
#15237=PRODUCT_RELATED_PRODUCT_CATEGORY(
'Linear Guide Rail - 15 mm, 220 mm Long',
'Linear Guide Rail - 15 mm, 220 mm Long',(#15293));
#15238=PRODUCT_RELATED_PRODUCT_CATEGORY(
'Sealed Ball Bearing - 10 x 30 x 9 mm',
'Sealed Ball Bearing - 10 x 30 x 9 mm',(#15294));
#15239=PRODUCT_RELATED_PRODUCT_CATEGORY('Inner ring','Inner ring',(#15295));
#15240=PRODUCT_RELATED_PRODUCT_CATEGORY('Outer ring','Outer ring',(#15296));
#15241=PRODUCT_RELATED_PRODUCT_CATEGORY('Balls','Balls',(#15297));
#15242=PRODUCT_RELATED_PRODUCT_CATEGORY('Cage','Cage',(#15298));
#15243=PRODUCT_RELATED_PRODUCT_CATEGORY('Seals 2RS','Seals 2RS',(#15299));
#15244=PRODUCT_RELATED_PRODUCT_CATEGORY('Driving crank','Driving crank',
(#15300));
#15245=PRODUCT_RELATED_PRODUCT_CATEGORY('Input crank and spindle',
'Input crank and spindle',(#15301));
#15246=PRODUCT_RELATED_PRODUCT_CATEGORY('Underside input grip',
'Underside input grip',(#15302));
#15247=PRODUCT_RELATED_PRODUCT_CATEGORY('Lower bearing sleeve',
'Lower bearing sleeve',(#15303));
#15248=PRODUCT_RELATED_PRODUCT_CATEGORY('Shaft collar','Shaft collar',(#15304));
#15249=PRODUCT_RELATED_PRODUCT_CATEGORY('Crank pin','Crank pin',(#15305));
#15250=PRODUCT_RELATED_PRODUCT_CATEGORY('Crank lower spacer',
'Crank lower spacer',(#15306));
#15251=PRODUCT_RELATED_PRODUCT_CATEGORY('Pin upper spacer',
'Pin upper spacer',(#15307));
#15252=PRODUCT_RELATED_PRODUCT_CATEGORY('Pin keeper','Pin keeper',(#15308));
#15253=PRODUCT_RELATED_PRODUCT_CATEGORY('Cap Screw - M4x16',
'Cap Screw - M4x16',(#15309));
#15254=PRODUCT_RELATED_PRODUCT_CATEGORY('Slotted lever','Slotted lever',
(#15310));
#15255=PRODUCT_RELATED_PRODUCT_CATEGORY('Slotted lever and spindle',
'Slotted lever and spindle',(#15311));
#15256=PRODUCT_RELATED_PRODUCT_CATEGORY('Lower bearing sleeve (1)',
'Lower bearing sleeve (1)',(#15312));
#15257=PRODUCT_RELATED_PRODUCT_CATEGORY('Shaft collar (1)',
'Shaft collar (1)',(#15313));
#15258=PRODUCT_RELATED_PRODUCT_CATEGORY('Lever output pin',
'Lever output pin',(#15314));
#15259=PRODUCT_RELATED_PRODUCT_CATEGORY('Lever output lower spacer',
'Lever output lower spacer',(#15315));
#15260=PRODUCT_RELATED_PRODUCT_CATEGORY('Pin upper spacer (1)',
'Pin upper spacer (1)',(#15316));
#15261=PRODUCT_RELATED_PRODUCT_CATEGORY('Pin keeper (1)',
'Pin keeper (1)',(#15317));
#15262=PRODUCT_RELATED_PRODUCT_CATEGORY('M4x4 collar screw',
'M4x4 collar screw',(#15318));
#15263=PRODUCT_RELATED_PRODUCT_CATEGORY('Sliding crank block',
'Sliding crank block',(#15319));
#15264=PRODUCT_RELATED_PRODUCT_CATEGORY('Captive sliding block',
'Captive sliding block',(#15320));
#15265=PRODUCT_RELATED_PRODUCT_CATEGORY('Output link','Output link',(#15321));
#15266=PRODUCT_RELATED_PRODUCT_CATEGORY('Connecting link',
'Connecting link',(#15322));
#15267=PRODUCT_RELATED_PRODUCT_CATEGORY('Link bushing','Link bushing',(#15323));
#15268=PRODUCT_RELATED_PRODUCT_CATEGORY('Link bushing (1)',
'Link bushing (1)',(#15324));
#15269=PRODUCT_RELATED_PRODUCT_CATEGORY('Guided output ram',
'Guided output ram',(#15325));
#15270=PRODUCT_RELATED_PRODUCT_CATEGORY('Ram table','Ram table',(#15326));
#15271=PRODUCT_RELATED_PRODUCT_CATEGORY('Ram pin','Ram pin',(#15327));
#15272=PRODUCT_RELATED_PRODUCT_CATEGORY('Ram lower spacer',
'Ram lower spacer',(#15328));
#15273=PRODUCT_RELATED_PRODUCT_CATEGORY('Pin upper spacer (2)',
'Pin upper spacer (2)',(#15329));
#15274=PRODUCT_RELATED_PRODUCT_CATEGORY('Pin keeper (2)',
'Pin keeper (2)',(#15330));
#15275=PRODUCT_RELATED_PRODUCT_CATEGORY(
'Flanged Linear Guide Carriage - 15 mm',
'Flanged Linear Guide Carriage - 15 mm',(#15331));
#15276=PRODUCT_RELATED_PRODUCT_CATEGORY('Block','Block',(#15332));
#15277=PRODUCT_RELATED_PRODUCT_CATEGORY('End cap +','End cap +',(#15333));
#15278=PRODUCT_RELATED_PRODUCT_CATEGORY('End cap','End cap',(#15334));
#15279=PRODUCT_RELATED_PRODUCT_CATEGORY('M5x14 Cap Screw',
'M5x14 Cap Screw',(#15335));
#15280=PRODUCT_RELATED_PRODUCT_CATEGORY('M4x10 Cap Screw',
'M4x10 Cap Screw',(#15336));
#15281=APPLICATION_PROTOCOL_DEFINITION('international standard',
'automotive_design',2009,#15282);
#15282=APPLICATION_CONTEXT(
'Core Data for Automotive Mechanical Design Process');
#15283=PRODUCT_CONTEXT('part definition',#15282,'mechanical');
#15284=PRODUCT('PAT-084','PAT-084',
'PAT-084',(#15283));
#15285=PRODUCT('Bearing base and output rail',
'Bearing base and output rail','Bearing base and output rail',(#15283));
#15286=PRODUCT('Base','Base','Base',(#15283));
#15287=PRODUCT('Foot strip','Foot strip','Foot strip',(#15283));
#15288=PRODUCT('Foot strip (1)','Foot strip (1)','Foot strip (1)',(#15283));
#15289=PRODUCT('Lever bearing post','Lever bearing post',
'Lever bearing post',(#15283));
#15290=PRODUCT('Bearing cap','Bearing cap','Bearing cap',(#15283));
#15291=PRODUCT('Crank bearing post','Crank bearing post',
'Crank bearing post',(#15283));
#15292=PRODUCT('Bearing cap (1)','Bearing cap (1)','Bearing cap (1)',(#15283));
#15293=PRODUCT('Linear Guide Rail - 15 mm, 220 mm Long',
'Linear Guide Rail - 15 mm, 220 mm Long',
'Linear Guide Rail - 15 mm, 220 mm Long',(#15283));
#15294=PRODUCT('Sealed Ball Bearing - 10 x 30 x 9 mm',
'Sealed Ball Bearing - 10 x 30 x 9 mm',
'Sealed Ball Bearing - 10 x 30 x 9 mm',(#15283));
#15295=PRODUCT('Inner ring','Inner ring','Inner ring',(#15283));
#15296=PRODUCT('Outer ring','Outer ring','Outer ring',(#15283));
#15297=PRODUCT('Balls','Balls','Balls',(#15283));
#15298=PRODUCT('Cage','Cage','Cage',(#15283));
#15299=PRODUCT('Seals 2RS','Seals 2RS','Seals 2RS',(#15283));
#15300=PRODUCT('Driving crank','Driving crank','Driving crank',(#15283));
#15301=PRODUCT('Input crank and spindle','Input crank and spindle',
'Input crank and spindle',(#15283));
#15302=PRODUCT('Underside input grip','Underside input grip',
'Underside input grip',(#15283));
#15303=PRODUCT('Lower bearing sleeve','Lower bearing sleeve',
'Lower bearing sleeve',(#15283));
#15304=PRODUCT('Shaft collar','Shaft collar','Shaft collar',(#15283));
#15305=PRODUCT('Crank pin','Crank pin','Crank pin',(#15283));
#15306=PRODUCT('Crank lower spacer','Crank lower spacer',
'Crank lower spacer',(#15283));
#15307=PRODUCT('Pin upper spacer','Pin upper spacer','Pin upper spacer',
(#15283));
#15308=PRODUCT('Pin keeper','Pin keeper','Pin keeper',(#15283));
#15309=PRODUCT('Cap Screw - M4x16','Cap Screw - M4x16',
'Cap Screw - M4x16',(#15283));
#15310=PRODUCT('Slotted lever','Slotted lever','Slotted lever',(#15283));
#15311=PRODUCT('Slotted lever and spindle','Slotted lever and spindle',
'Slotted lever and spindle',(#15283));
#15312=PRODUCT('Lower bearing sleeve (1)','Lower bearing sleeve (1)',
'Lower bearing sleeve (1)',(#15283));
#15313=PRODUCT('Shaft collar (1)','Shaft collar (1)','Shaft collar (1)',(#15283));
#15314=PRODUCT('Lever output pin','Lever output pin','Lever output pin',
(#15283));
#15315=PRODUCT('Lever output lower spacer','Lever output lower spacer',
'Lever output lower spacer',(#15283));
#15316=PRODUCT('Pin upper spacer (1)','Pin upper spacer (1)',
'Pin upper spacer (1)',(#15283));
#15317=PRODUCT('Pin keeper (1)','Pin keeper (1)','Pin keeper (1)',(#15283));
#15318=PRODUCT('M4x4 collar screw','M4x4 collar screw',
'M4x4 collar screw',(#15283));
#15319=PRODUCT('Sliding crank block','Sliding crank block',
'Sliding crank block',(#15283));
#15320=PRODUCT('Captive sliding block','Captive sliding block',
'Captive sliding block',(#15283));
#15321=PRODUCT('Output link','Output link','Output link',(#15283));
#15322=PRODUCT('Connecting link','Connecting link','Connecting link',(#15283));
#15323=PRODUCT('Link bushing','Link bushing','Link bushing',(#15283));
#15324=PRODUCT('Link bushing (1)','Link bushing (1)','Link bushing (1)',(#15283));
#15325=PRODUCT('Guided output ram','Guided output ram',
'Guided output ram',(#15283));
#15326=PRODUCT('Ram table','Ram table','Ram table',(#15283));
#15327=PRODUCT('Ram pin','Ram pin','Ram pin',(#15283));
#15328=PRODUCT('Ram lower spacer','Ram lower spacer','Ram lower spacer',
(#15283));
#15329=PRODUCT('Pin upper spacer (2)','Pin upper spacer (2)',
'Pin upper spacer (2)',(#15283));
#15330=PRODUCT('Pin keeper (2)','Pin keeper (2)','Pin keeper (2)',(#15283));
#15331=PRODUCT('Flanged Linear Guide Carriage - 15 mm',
'Flanged Linear Guide Carriage - 15 mm',
'Flanged Linear Guide Carriage - 15 mm',(#15283));
#15332=PRODUCT('Block','Block','Block',(#15283));
#15333=PRODUCT('End cap +','End cap +','End cap +',(#15283));
#15334=PRODUCT('End cap','End cap','End cap',(#15283));
#15335=PRODUCT('M5x14 Cap Screw','M5x14 Cap Screw','M5x14 Cap Screw',(#15283));
#15336=PRODUCT('M4x10 Cap Screw','M4x10 Cap Screw','M4x10 Cap Screw',(#15283));
#15337=PRESENTATION_STYLE_ASSIGNMENT((#15343));
#15338=PRESENTATION_STYLE_ASSIGNMENT((#15344));
#15339=PRESENTATION_STYLE_ASSIGNMENT((#15345));
#15340=PRESENTATION_STYLE_ASSIGNMENT((#15346));
#15341=PRESENTATION_STYLE_ASSIGNMENT((#15347));
#15342=PRESENTATION_STYLE_ASSIGNMENT((#15348));
#15343=SURFACE_STYLE_USAGE(.BOTH.,#15349);
#15344=SURFACE_STYLE_USAGE(.BOTH.,#15350);
#15345=SURFACE_STYLE_USAGE(.BOTH.,#15351);
#15346=SURFACE_STYLE_USAGE(.BOTH.,#15352);
#15347=SURFACE_STYLE_USAGE(.BOTH.,#15353);
#15348=SURFACE_STYLE_USAGE(.BOTH.,#15354);
#15349=SURFACE_SIDE_STYLE('',(#15355));
#15350=SURFACE_SIDE_STYLE('',(#15356));
#15351=SURFACE_SIDE_STYLE('',(#15357));
#15352=SURFACE_SIDE_STYLE('',(#15358));
#15353=SURFACE_SIDE_STYLE('',(#15359));
#15354=SURFACE_SIDE_STYLE('',(#15360));
#15355=SURFACE_STYLE_FILL_AREA(#15361);
#15356=SURFACE_STYLE_FILL_AREA(#15362);
#15357=SURFACE_STYLE_FILL_AREA(#15363);
#15358=SURFACE_STYLE_FILL_AREA(#15364);
#15359=SURFACE_STYLE_FILL_AREA(#15365);
#15360=SURFACE_STYLE_FILL_AREA(#15366);
#15361=FILL_AREA_STYLE('Steel - Satin',(#15367));
#15362=FILL_AREA_STYLE('CAD Library Painted - Deep blue',(#15368));
#15363=FILL_AREA_STYLE('CAD Library Painted - Steel gray',(#15369));
#15364=FILL_AREA_STYLE('CAD Library Painted - Engineering blue',(#15370));
#15365=FILL_AREA_STYLE('CAD Library Painted - Graphite',(#15371));
#15366=FILL_AREA_STYLE('CAD Library Painted - Light blue',(#15372));
#15367=FILL_AREA_STYLE_COLOUR('Steel - Satin',#15373);
#15368=FILL_AREA_STYLE_COLOUR('CAD Library Painted - Deep blue',#15374);
#15369=FILL_AREA_STYLE_COLOUR('CAD Library Painted - Steel gray',#15375);
#15370=FILL_AREA_STYLE_COLOUR('CAD Library Painted - Engineering blue',
#15376);
#15371=FILL_AREA_STYLE_COLOUR('CAD Library Painted - Graphite',#15377);
#15372=FILL_AREA_STYLE_COLOUR('CAD Library Painted - Light blue',#15378);
#15373=COLOUR_RGB('Steel - Satin',0.627450980392157,0.627450980392157,0.627450980392157);
#15374=COLOUR_RGB('CAD Library Painted - Deep blue',0.0784313725490196,
0.203921568627451,0.349019607843137);
#15375=COLOUR_RGB('CAD Library Painted - Steel gray',0.592156862745098,
0.631372549019608,0.67843137254902);
#15376=COLOUR_RGB('CAD Library Painted - Engineering blue',0.12156862745098,
0.356862745098039,0.6);
#15377=COLOUR_RGB('CAD Library Painted - Graphite',0.168627450980392,0.192156862745098,
0.231372549019608);
#15378=COLOUR_RGB('CAD Library Painted - Light blue',0.286274509803922,
0.552941176470588,0.780392156862745);
#15379=COLOUR_RGB('Dark Blue',0.08,0.2,0.34);
#15380=FILL_AREA_STYLE_COLOUR('',#15379);
#15381=FILL_AREA_STYLE('',(#15380));
#15382=SURFACE_STYLE_FILL_AREA(#15381);
#15383=SURFACE_SIDE_STYLE('',(#15382));
#15384=SURFACE_STYLE_USAGE(.BOTH.,#15383);
#15385=PRESENTATION_STYLE_ASSIGNMENT((#15384));
#15386=COLOUR_RGB('Light Blue',0.38,0.62,0.78);
#15387=FILL_AREA_STYLE_COLOUR('',#15386);
#15388=FILL_AREA_STYLE('',(#15387));
#15389=SURFACE_STYLE_FILL_AREA(#15388);
#15390=SURFACE_SIDE_STYLE('',(#15389));
#15391=SURFACE_STYLE_USAGE(.BOTH.,#15390);
#15392=PRESENTATION_STYLE_ASSIGNMENT((#15391));
#15393=COLOUR_RGB('Sky Blue',0.24,0.69,0.87);
#15394=FILL_AREA_STYLE_COLOUR('',#15393);
#15395=FILL_AREA_STYLE('',(#15394));
#15396=SURFACE_STYLE_FILL_AREA(#15395);
#15397=SURFACE_SIDE_STYLE('',(#15396));
#15398=SURFACE_STYLE_USAGE(.BOTH.,#15397);
#15399=PRESENTATION_STYLE_ASSIGNMENT((#15398));
#15400=COLOUR_RGB('Grey',0.48,0.52,0.57);
#15401=FILL_AREA_STYLE_COLOUR('',#15400);
#15402=FILL_AREA_STYLE('',(#15401));
#15403=SURFACE_STYLE_FILL_AREA(#15402);
#15404=SURFACE_SIDE_STYLE('',(#15403));
#15405=SURFACE_STYLE_USAGE(.BOTH.,#15404);
#15406=PRESENTATION_STYLE_ASSIGNMENT((#15405));
#15407=COLOUR_RGB('Black',0.12,0.14,0.17);
#15408=FILL_AREA_STYLE_COLOUR('',#15407);
#15409=FILL_AREA_STYLE('',(#15408));
#15410=SURFACE_STYLE_FILL_AREA(#15409);
#15411=SURFACE_SIDE_STYLE('',(#15410));
#15412=SURFACE_STYLE_USAGE(.BOTH.,#15411);
#15413=PRESENTATION_STYLE_ASSIGNMENT((#15412));
#15414=COLOUR_RGB('Off White',0.89,0.88,0.83);
#15415=FILL_AREA_STYLE_COLOUR('',#15414);
#15416=FILL_AREA_STYLE('',(#15415));
#15417=SURFACE_STYLE_FILL_AREA(#15416);
#15418=SURFACE_SIDE_STYLE('',(#15417));
#15419=SURFACE_STYLE_USAGE(.BOTH.,#15418);
#15420=PRESENTATION_STYLE_ASSIGNMENT((#15419));
ENDSEC;
END-ISO-10303-21;
